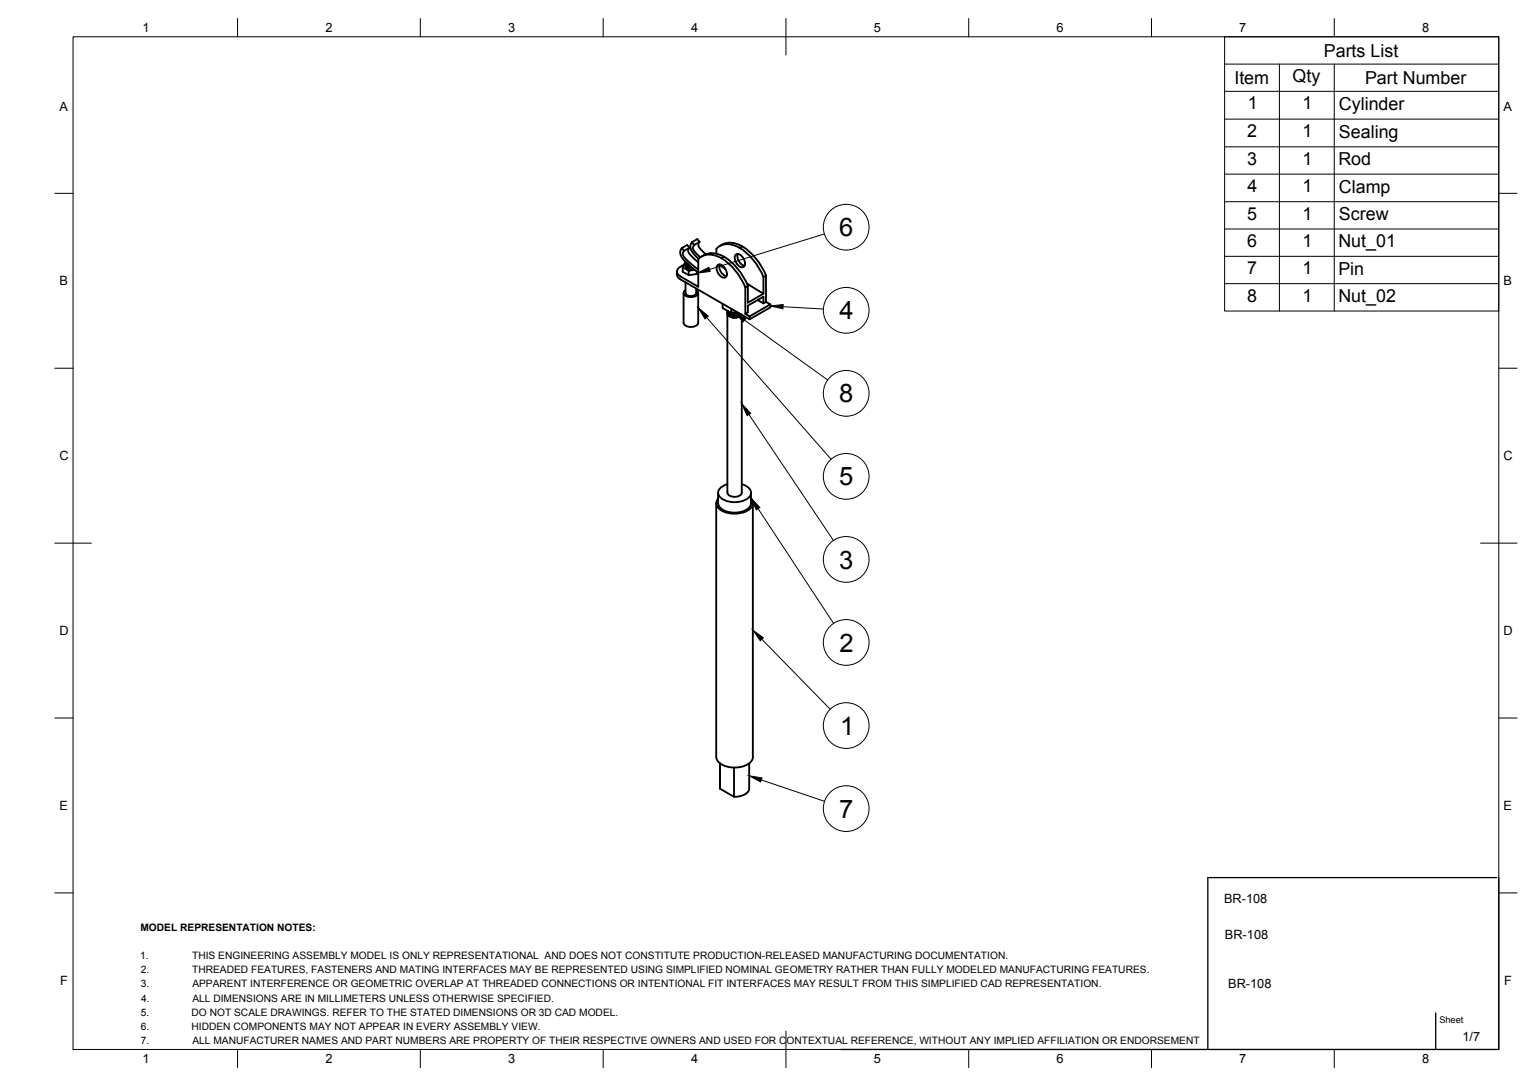
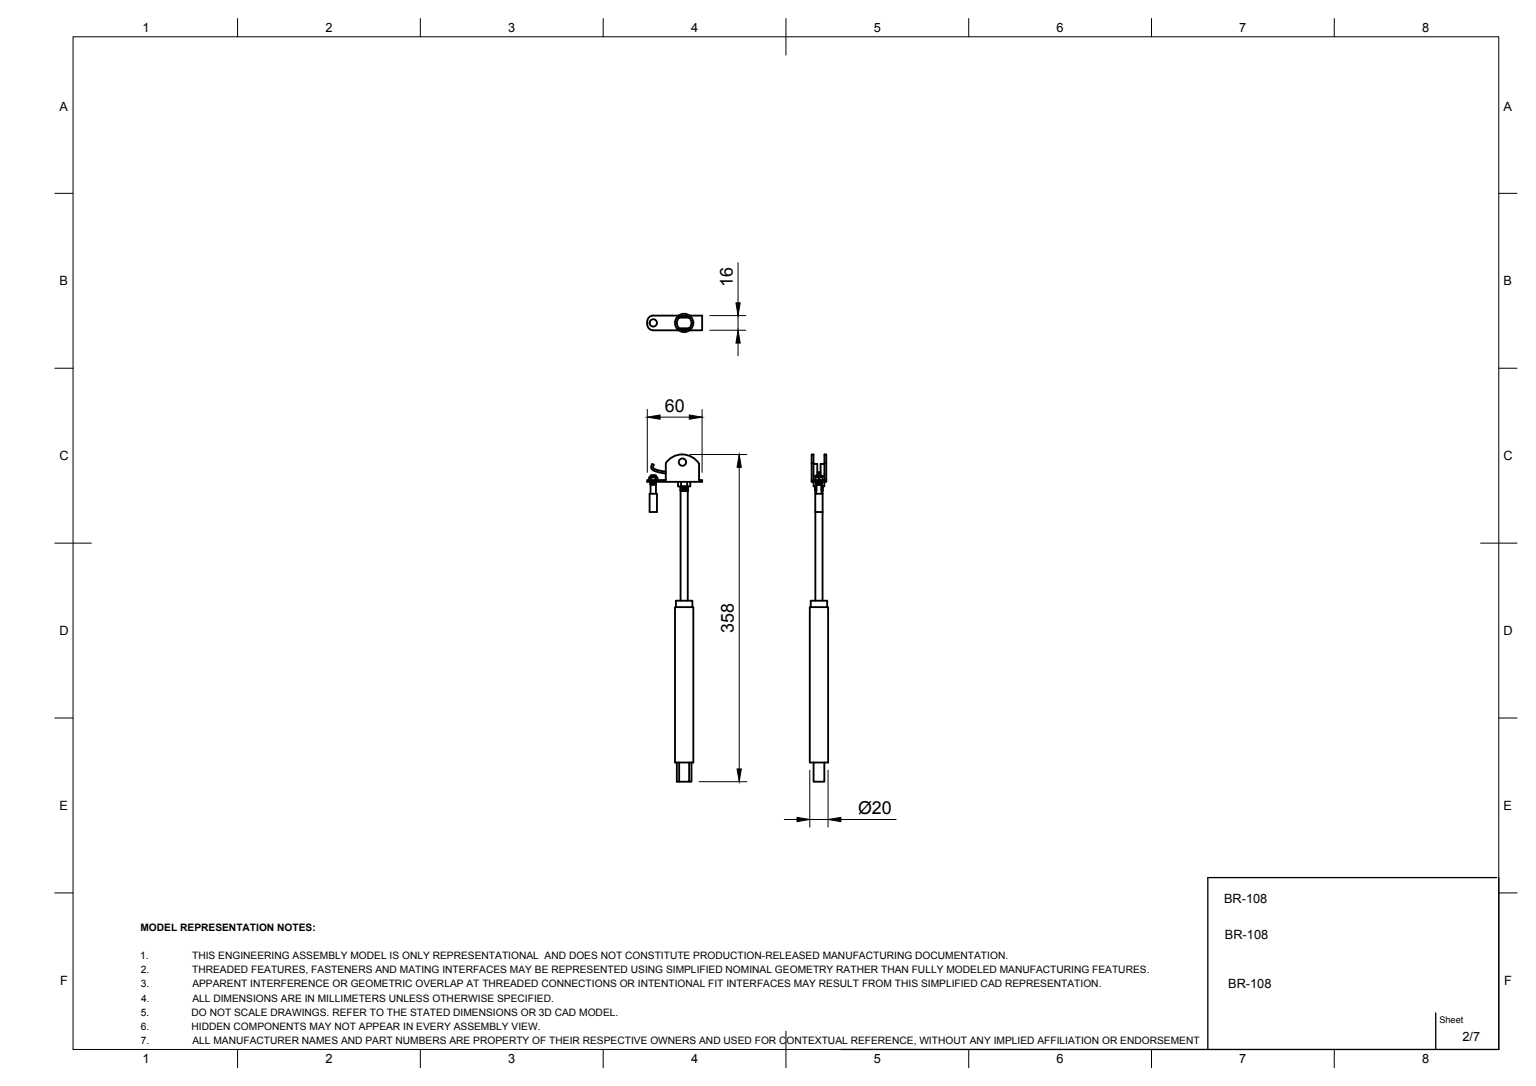
ISO-10303-21;
HEADER;
/* Generated by software containing ST-Developer
 * from STEP Tools, Inc. (www.steptools.com) 
 */

FILE_DESCRIPTION(
/* description */ (''),
/* implementation_level */ '2;1');

FILE_NAME(
/* name */ 'BR-108.step',
/* time_stamp */ '2026-11-14T03:52:36-08:00',
/* author */ (''),
/* organization */ (''),
/* preprocessor_version */ 'ST-DEVELOPER v20.2',
/* originating_system */ 'Autodesk Translation Framework v15.17.0.0',
/* authorisation */ '');

FILE_SCHEMA (('AUTOMOTIVE_DESIGN { 1 0 10303 214 3 1 1 }'));
ENDSEC;

DATA;
#10=MECHANICAL_DESIGN_GEOMETRIC_PRESENTATION_REPRESENTATION('',(#191,#192,
#193,#194,#195,#196,#197,#198),#19443);
#11=ITEM_DEFINED_TRANSFORMATION($,$,#2116,#2258);
#12=ITEM_DEFINED_TRANSFORMATION($,$,#2125,#2259);
#13=ITEM_DEFINED_TRANSFORMATION($,$,#2131,#2260);
#14=ITEM_DEFINED_TRANSFORMATION($,$,#2150,#2261);
#15=ITEM_DEFINED_TRANSFORMATION($,$,#2195,#2262);
#16=ITEM_DEFINED_TRANSFORMATION($,$,#2220,#2263);
#17=ITEM_DEFINED_TRANSFORMATION($,$,#2232,#2264);
#18=ITEM_DEFINED_TRANSFORMATION($,$,#2246,#2265);
#19=(
REPRESENTATION_RELATIONSHIP($,$,#19475,#19474)
REPRESENTATION_RELATIONSHIP_WITH_TRANSFORMATION(#11)
SHAPE_REPRESENTATION_RELATIONSHIP()
);
#20=(
REPRESENTATION_RELATIONSHIP($,$,#19476,#19474)
REPRESENTATION_RELATIONSHIP_WITH_TRANSFORMATION(#12)
SHAPE_REPRESENTATION_RELATIONSHIP()
);
#21=(
REPRESENTATION_RELATIONSHIP($,$,#19477,#19474)
REPRESENTATION_RELATIONSHIP_WITH_TRANSFORMATION(#13)
SHAPE_REPRESENTATION_RELATIONSHIP()
);
#22=(
REPRESENTATION_RELATIONSHIP($,$,#19478,#19474)
REPRESENTATION_RELATIONSHIP_WITH_TRANSFORMATION(#14)
SHAPE_REPRESENTATION_RELATIONSHIP()
);
#23=(
REPRESENTATION_RELATIONSHIP($,$,#19479,#19474)
REPRESENTATION_RELATIONSHIP_WITH_TRANSFORMATION(#15)
SHAPE_REPRESENTATION_RELATIONSHIP()
);
#24=(
REPRESENTATION_RELATIONSHIP($,$,#19480,#19474)
REPRESENTATION_RELATIONSHIP_WITH_TRANSFORMATION(#16)
SHAPE_REPRESENTATION_RELATIONSHIP()
);
#25=(
REPRESENTATION_RELATIONSHIP($,$,#19481,#19474)
REPRESENTATION_RELATIONSHIP_WITH_TRANSFORMATION(#17)
SHAPE_REPRESENTATION_RELATIONSHIP()
);
#26=(
REPRESENTATION_RELATIONSHIP($,$,#19482,#19474)
REPRESENTATION_RELATIONSHIP_WITH_TRANSFORMATION(#18)
SHAPE_REPRESENTATION_RELATIONSHIP()
);
#27=CONTEXT_DEPENDENT_SHAPE_REPRESENTATION(#19,#19466);
#28=CONTEXT_DEPENDENT_SHAPE_REPRESENTATION(#20,#19467);
#29=CONTEXT_DEPENDENT_SHAPE_REPRESENTATION(#21,#19468);
#30=CONTEXT_DEPENDENT_SHAPE_REPRESENTATION(#22,#19469);
#31=CONTEXT_DEPENDENT_SHAPE_REPRESENTATION(#23,#19470);
#32=CONTEXT_DEPENDENT_SHAPE_REPRESENTATION(#24,#19471);
#33=CONTEXT_DEPENDENT_SHAPE_REPRESENTATION(#25,#19472);
#34=CONTEXT_DEPENDENT_SHAPE_REPRESENTATION(#26,#19473);
#35=NEXT_ASSEMBLY_USAGE_OCCURRENCE('Cylinder:1','Cylinder:1',
'Cylinder:1',#19484,#19485,'Cylinder:1');
#36=NEXT_ASSEMBLY_USAGE_OCCURRENCE('Sealing:1','Sealing:1','Sealing:1',
#19484,#19486,'Sealing:1');
#37=NEXT_ASSEMBLY_USAGE_OCCURRENCE('Rod:1','Rod:1','Rod:1',#19484,#19487,
'Rod:1');
#38=NEXT_ASSEMBLY_USAGE_OCCURRENCE('Clamp:1','Clamp:1','Clamp:1',#19484,
#19488,'Clamp:1');
#39=NEXT_ASSEMBLY_USAGE_OCCURRENCE('Screw:1','Screw:1','Screw:1',#19484,
#19489,'Screw:1');
#40=NEXT_ASSEMBLY_USAGE_OCCURRENCE('Nut_01:1','Nut_01:1','Nut_01:1',#19484,
#19490,'Nut_01:1');
#41=NEXT_ASSEMBLY_USAGE_OCCURRENCE('Pin:1','Pin:1','Pin:1',#19484,#19491,
'Pin:1');
#42=NEXT_ASSEMBLY_USAGE_OCCURRENCE('Nut_02:1','Nut_02:1','Nut_02:1',#19484,
#19492,'Nut_02:1');
#43=B_SPLINE_SURFACE_WITH_KNOTS('',3,3,((#8954,#8955,#8956,#8957,#8958,
#8959,#8960,#8961,#8962,#8963,#8964,#8965,#8966,#8967,#8968,#8969,#8970,
#8971,#8972,#8973,#8974,#8975,#8976,#8977,#8978,#8979,#8980,#8981,#8982,
#8983,#8984,#8985,#8986,#8987,#8988,#8989,#8990,#8991,#8992,#8993,#8994,
#8995,#8996,#8997,#8998,#8999,#9000,#9001,#9002,#9003,#9004,#9005,#9006,
#9007,#9008,#9009),(#9010,#9011,#9012,#9013,#9014,#9015,#9016,#9017,#9018,
#9019,#9020,#9021,#9022,#9023,#9024,#9025,#9026,#9027,#9028,#9029,#9030,
#9031,#9032,#9033,#9034,#9035,#9036,#9037,#9038,#9039,#9040,#9041,#9042,
#9043,#9044,#9045,#9046,#9047,#9048,#9049,#9050,#9051,#9052,#9053,#9054,
#9055,#9056,#9057,#9058,#9059,#9060,#9061,#9062,#9063,#9064,#9065),(#9066,
#9067,#9068,#9069,#9070,#9071,#9072,#9073,#9074,#9075,#9076,#9077,#9078,
#9079,#9080,#9081,#9082,#9083,#9084,#9085,#9086,#9087,#9088,#9089,#9090,
#9091,#9092,#9093,#9094,#9095,#9096,#9097,#9098,#9099,#9100,#9101,#9102,
#9103,#9104,#9105,#9106,#9107,#9108,#9109,#9110,#9111,#9112,#9113,#9114,
#9115,#9116,#9117,#9118,#9119,#9120,#9121),(#9122,#9123,#9124,#9125,#9126,
#9127,#9128,#9129,#9130,#9131,#9132,#9133,#9134,#9135,#9136,#9137,#9138,
#9139,#9140,#9141,#9142,#9143,#9144,#9145,#9146,#9147,#9148,#9149,#9150,
#9151,#9152,#9153,#9154,#9155,#9156,#9157,#9158,#9159,#9160,#9161,#9162,
#9163,#9164,#9165,#9166,#9167,#9168,#9169,#9170,#9171,#9172,#9173,#9174,
#9175,#9176,#9177)),.UNSPECIFIED.,.F.,.F.,.F.,(4,4),(4,1,1,1,1,1,1,1,1,
1,1,1,1,1,1,1,1,1,1,1,1,1,1,1,1,1,1,1,1,1,1,1,1,1,1,1,1,1,1,1,1,1,1,1,1,
1,1,1,1,1,1,1,1,4),(-0.000657437329809864,0.0823479142293904),(8.31473274985805,
9.30202867542319,10.2893246009883,11.2766205265535,12.2639164521186,13.2512123776837,
14.2385083032489,15.225804228814,16.2131001543792,17.2003960799443,18.1876920055094,
19.1749879310746,20.1622838566397,21.1495797822049,22.13687570777,23.1241716333351,
24.1114675589003,25.0987634844654,26.0860594100306,27.0733553355957,28.0606512611608,
29.047947186726,30.0352431122911,31.0225390378563,32.0098349634214,32.9971308889865,
33.9844268145517,34.9717227401168,35.959018665682,36.9463145912471,37.9336105168122,
38.9209064423774,39.9082023679425,40.8954982935077,41.8827942190728,42.8700901446379,
43.8573860702031,44.8446819957682,45.8319779213334,46.8192738468985,47.8065697724636,
48.7938656980288,49.7811616235939,50.7684575491591,51.7557534747242,52.7430494002893,
53.7303453258545,54.7176412514196,55.7049371769848,56.6922331025499,57.679529028115,
58.6668249536802,59.6541208792453,60.6420742421403),.UNSPECIFIED.);
#44=B_SPLINE_SURFACE_WITH_KNOTS('',3,3,((#9461,#9462,#9463,#9464,#9465,
#9466,#9467,#9468,#9469,#9470,#9471,#9472,#9473,#9474,#9475,#9476,#9477,
#9478,#9479,#9480,#9481,#9482,#9483,#9484,#9485,#9486,#9487,#9488,#9489,
#9490,#9491,#9492,#9493,#9494,#9495,#9496,#9497,#9498,#9499,#9500,#9501,
#9502,#9503,#9504,#9505,#9506,#9507,#9508,#9509,#9510,#9511,#9512,#9513,
#9514,#9515,#9516),(#9517,#9518,#9519,#9520,#9521,#9522,#9523,#9524,#9525,
#9526,#9527,#9528,#9529,#9530,#9531,#9532,#9533,#9534,#9535,#9536,#9537,
#9538,#9539,#9540,#9541,#9542,#9543,#9544,#9545,#9546,#9547,#9548,#9549,
#9550,#9551,#9552,#9553,#9554,#9555,#9556,#9557,#9558,#9559,#9560,#9561,
#9562,#9563,#9564,#9565,#9566,#9567,#9568,#9569,#9570,#9571,#9572),(#9573,
#9574,#9575,#9576,#9577,#9578,#9579,#9580,#9581,#9582,#9583,#9584,#9585,
#9586,#9587,#9588,#9589,#9590,#9591,#9592,#9593,#9594,#9595,#9596,#9597,
#9598,#9599,#9600,#9601,#9602,#9603,#9604,#9605,#9606,#9607,#9608,#9609,
#9610,#9611,#9612,#9613,#9614,#9615,#9616,#9617,#9618,#9619,#9620,#9621,
#9622,#9623,#9624,#9625,#9626,#9627,#9628),(#9629,#9630,#9631,#9632,#9633,
#9634,#9635,#9636,#9637,#9638,#9639,#9640,#9641,#9642,#9643,#9644,#9645,
#9646,#9647,#9648,#9649,#9650,#9651,#9652,#9653,#9654,#9655,#9656,#9657,
#9658,#9659,#9660,#9661,#9662,#9663,#9664,#9665,#9666,#9667,#9668,#9669,
#9670,#9671,#9672,#9673,#9674,#9675,#9676,#9677,#9678,#9679,#9680,#9681,
#9682,#9683,#9684)),.UNSPECIFIED.,.F.,.F.,.F.,(4,4),(4,1,1,1,1,1,1,1,1,
1,1,1,1,1,1,1,1,1,1,1,1,1,1,1,1,1,1,1,1,1,1,1,1,1,1,1,1,1,1,1,1,1,1,1,1,
1,1,1,1,1,1,1,1,4),(-0.00040521448804481,0.0826859266002323),(11.6145409068929,
12.6025101533199,13.589806078885,14.5771020044501,15.5643979300153,16.5516938555804,
17.5389897811456,18.5262857067107,19.5135816322758,20.500877557841,21.4881734834061,
22.4754694089713,23.4627653345364,24.4500612601015,25.4373571856667,26.4246531112318,
27.411949036797,28.3992449623621,29.3865408879273,30.3738368134924,31.3611327390575,
32.3484286646227,33.3357245901878,34.323020515753,35.3103164413181,36.2976123668832,
37.2849082924484,38.2722042180135,39.2595001435787,40.2467960691438,41.2340919947089,
42.2213879202741,43.2086838458392,44.1959797714044,45.1832756969695,46.1705716225347,
47.1578675480998,48.1451634736649,49.1324593992301,50.1197553247952,51.1070512503604,
52.0943471759255,53.0816431014906,54.0689390270558,55.0562349526209,56.0435308781861,
57.0308268037512,58.0181227293163,59.0054186548815,59.9927145804466,60.9800105060118,
61.9673064315769,62.954602357142,63.9418982827072),.UNSPECIFIED.);
#45=B_SPLINE_SURFACE_WITH_KNOTS('',5,1,((#10544,#10545),(#10546,#10547),
(#10548,#10549),(#10550,#10551),(#10552,#10553),(#10554,#10555),(#10556,
#10557),(#10558,#10559),(#10560,#10561),(#10562,#10563),(#10564,#10565),
(#10566,#10567),(#10568,#10569),(#10570,#10571),(#10572,#10573),(#10574,
#10575),(#10576,#10577),(#10578,#10579),(#10580,#10581),(#10582,#10583),
(#10584,#10585),(#10586,#10587),(#10588,#10589),(#10590,#10591),(#10592,
#10593)),.UNSPECIFIED.,.F.,.F.,.F.,(6,1,1,1,1,1,1,1,1,1,1,1,1,1,1,1,1,1,
1,1,6),(2,2),(0.,0.05,0.1,0.15,0.2,0.25,0.3,0.35,0.4,0.45,0.5,0.55,0.6,
0.65,0.7,0.75,0.8,0.85,0.9,0.95,0.997783576468117),(0.,2.28),
 .UNSPECIFIED.);
#46=B_SPLINE_SURFACE_WITH_KNOTS('',3,1,((#10795,#10796),(#10797,#10798),
(#10799,#10800),(#10801,#10802),(#10803,#10804),(#10805,#10806),(#10807,
#10808),(#10809,#10810),(#10811,#10812),(#10813,#10814),(#10815,#10816),
(#10817,#10818),(#10819,#10820),(#10821,#10822),(#10823,#10824),(#10825,
#10826),(#10827,#10828),(#10829,#10830),(#10831,#10832),(#10833,#10834),
(#10835,#10836),(#10837,#10838)),.UNSPECIFIED.,.F.,.F.,.F.,(4,3,3,3,3,3,
3,4),(2,2),(-1.,-0.911417181577933,-0.82714074028049,-0.742907558806874,
-0.633245293286216,-0.436057375062027,-0.250000004296482,-0.000486150394329065),
(0.,2.28),.UNSPECIFIED.);
#47=B_SPLINE_SURFACE_WITH_KNOTS('',3,3,((#18367,#18368,#18369,#18370,#18371,
#18372,#18373,#18374,#18375,#18376,#18377,#18378,#18379,#18380,#18381,#18382,
#18383,#18384,#18385,#18386,#18387,#18388,#18389,#18390,#18391,#18392,#18393,
#18394,#18395,#18396,#18397,#18398,#18399,#18400,#18401,#18402,#18403,#18404,
#18405,#18406,#18407,#18408,#18409,#18410,#18411,#18412,#18413,#18414,#18415,
#18416,#18417,#18418,#18419,#18420,#18421,#18422,#18423,#18424,#18425,#18426,
#18427,#18428,#18429,#18430,#18431,#18432,#18433,#18434),(#18435,#18436,
#18437,#18438,#18439,#18440,#18441,#18442,#18443,#18444,#18445,#18446,#18447,
#18448,#18449,#18450,#18451,#18452,#18453,#18454,#18455,#18456,#18457,#18458,
#18459,#18460,#18461,#18462,#18463,#18464,#18465,#18466,#18467,#18468,#18469,
#18470,#18471,#18472,#18473,#18474,#18475,#18476,#18477,#18478,#18479,#18480,
#18481,#18482,#18483,#18484,#18485,#18486,#18487,#18488,#18489,#18490,#18491,
#18492,#18493,#18494,#18495,#18496,#18497,#18498,#18499,#18500,#18501,#18502),
(#18503,#18504,#18505,#18506,#18507,#18508,#18509,#18510,#18511,#18512,
#18513,#18514,#18515,#18516,#18517,#18518,#18519,#18520,#18521,#18522,#18523,
#18524,#18525,#18526,#18527,#18528,#18529,#18530,#18531,#18532,#18533,#18534,
#18535,#18536,#18537,#18538,#18539,#18540,#18541,#18542,#18543,#18544,#18545,
#18546,#18547,#18548,#18549,#18550,#18551,#18552,#18553,#18554,#18555,#18556,
#18557,#18558,#18559,#18560,#18561,#18562,#18563,#18564,#18565,#18566,#18567,
#18568,#18569,#18570),(#18571,#18572,#18573,#18574,#18575,#18576,#18577,
#18578,#18579,#18580,#18581,#18582,#18583,#18584,#18585,#18586,#18587,#18588,
#18589,#18590,#18591,#18592,#18593,#18594,#18595,#18596,#18597,#18598,#18599,
#18600,#18601,#18602,#18603,#18604,#18605,#18606,#18607,#18608,#18609,#18610,
#18611,#18612,#18613,#18614,#18615,#18616,#18617,#18618,#18619,#18620,#18621,
#18622,#18623,#18624,#18625,#18626,#18627,#18628,#18629,#18630,#18631,#18632,
#18633,#18634,#18635,#18636,#18637,#18638)),.UNSPECIFIED.,.F.,.F.,.F.,(4,
4),(4,1,1,1,1,1,1,1,1,1,1,1,1,1,1,1,1,1,1,1,1,1,1,1,1,1,1,1,1,1,1,1,1,1,
1,1,1,1,1,1,1,1,1,1,1,1,1,1,1,1,1,1,1,1,1,1,1,1,1,1,1,1,1,1,1,4),(-0.000501830952949241,
0.0663068519672736),(8.30747755240111,9.30594664850426,10.3044157446074,
11.3028848407106,12.3013539368137,13.2998230329169,14.29829212902,15.2967612251232,
16.2952303212263,17.2936994173295,18.2921685134326,19.2906376095358,20.2891067056389,
21.2875758017421,22.2860448978452,23.2845139939484,24.2829830900515,25.2814521861547,
26.2799212822578,27.278390378361,28.2768594744641,29.2753285705673,30.2737976666704,
31.2722667627736,32.2707358588767,33.2692049549799,34.267674051083,35.2661431471862,
36.2646122432893,37.2630813393925,38.2615504354956,39.2600195315988,40.258488627702,
41.2569577238051,42.2554268199083,43.2538959160114,44.2523650121146,45.2508341082177,
46.2493032043209,47.247772300424,48.2462413965272,49.2447104926303,50.2431795887335,
51.2416486848366,52.2401177809398,53.2385868770429,54.2370559731461,55.2355250692492,
56.2339941653524,57.2324632614555,58.2309323575587,59.2294014536618,60.227870549765,
61.2263396458681,62.2248087419713,63.2232778380744,64.2217469341776,65.2202160302807,
66.2186851263839,67.217154222487,68.2156233185902,69.2140924146934,70.2125615107965,
71.2110306068997,72.2094997030028,73.208470630059),.UNSPECIFIED.);
#48=B_SPLINE_SURFACE_WITH_KNOTS('',3,3,((#18916,#18917,#18918,#18919,#18920,
#18921,#18922,#18923,#18924,#18925,#18926,#18927,#18928,#18929,#18930,#18931,
#18932,#18933,#18934,#18935,#18936,#18937,#18938,#18939,#18940,#18941,#18942,
#18943,#18944,#18945,#18946,#18947,#18948,#18949,#18950,#18951,#18952,#18953,
#18954,#18955,#18956,#18957,#18958,#18959,#18960,#18961,#18962,#18963,#18964,
#18965,#18966,#18967,#18968,#18969,#18970,#18971,#18972,#18973,#18974,#18975,
#18976,#18977,#18978,#18979,#18980,#18981,#18982,#18983),(#18984,#18985,
#18986,#18987,#18988,#18989,#18990,#18991,#18992,#18993,#18994,#18995,#18996,
#18997,#18998,#18999,#19000,#19001,#19002,#19003,#19004,#19005,#19006,#19007,
#19008,#19009,#19010,#19011,#19012,#19013,#19014,#19015,#19016,#19017,#19018,
#19019,#19020,#19021,#19022,#19023,#19024,#19025,#19026,#19027,#19028,#19029,
#19030,#19031,#19032,#19033,#19034,#19035,#19036,#19037,#19038,#19039,#19040,
#19041,#19042,#19043,#19044,#19045,#19046,#19047,#19048,#19049,#19050,#19051),
(#19052,#19053,#19054,#19055,#19056,#19057,#19058,#19059,#19060,#19061,
#19062,#19063,#19064,#19065,#19066,#19067,#19068,#19069,#19070,#19071,#19072,
#19073,#19074,#19075,#19076,#19077,#19078,#19079,#19080,#19081,#19082,#19083,
#19084,#19085,#19086,#19087,#19088,#19089,#19090,#19091,#19092,#19093,#19094,
#19095,#19096,#19097,#19098,#19099,#19100,#19101,#19102,#19103,#19104,#19105,
#19106,#19107,#19108,#19109,#19110,#19111,#19112,#19113,#19114,#19115,#19116,
#19117,#19118,#19119),(#19120,#19121,#19122,#19123,#19124,#19125,#19126,
#19127,#19128,#19129,#19130,#19131,#19132,#19133,#19134,#19135,#19136,#19137,
#19138,#19139,#19140,#19141,#19142,#19143,#19144,#19145,#19146,#19147,#19148,
#19149,#19150,#19151,#19152,#19153,#19154,#19155,#19156,#19157,#19158,#19159,
#19160,#19161,#19162,#19163,#19164,#19165,#19166,#19167,#19168,#19169,#19170,
#19171,#19172,#19173,#19174,#19175,#19176,#19177,#19178,#19179,#19180,#19181,
#19182,#19183,#19184,#19185,#19186,#19187)),.UNSPECIFIED.,.F.,.F.,.F.,(4,
4),(4,1,1,1,1,1,1,1,1,1,1,1,1,1,1,1,1,1,1,1,1,1,1,1,1,1,1,1,1,1,1,1,1,1,
1,1,1,1,1,1,1,1,1,1,1,1,1,1,1,1,1,1,1,1,1,1,1,1,1,1,1,1,1,1,1,4),(-0.000439241290791206,
0.0663646041699065),(11.6145150418495,12.6135019439215,13.6119710400246,
14.6104401361278,15.6089092322309,16.6073783283341,17.6058474244372,18.6043165205404,
19.6027856166435,20.6012547127467,21.5997238088498,22.598192904953,23.5966620010561,
24.5951310971593,25.5936001932624,26.5920692893656,27.5905383854687,28.5890074815719,
29.5874765776751,30.5859456737782,31.5844147698814,32.5828838659845,33.5813529620877,
34.5798220581908,35.578291154294,36.5767602503971,37.5752293465003,38.5736984426034,
39.5721675387066,40.5706366348097,41.5691057309129,42.567574827016,43.5660439231192,
44.5645130192223,45.5629821153255,46.5614512114286,47.5599203075318,48.5583894036349,
49.5568584997381,50.5553275958412,51.5537966919444,52.5522657880475,53.5507348841507,
54.5492039802538,55.547673076357,56.5461421724601,57.5446112685633,58.5430803646665,
59.5415494607696,60.5400185568728,61.5384876529759,62.5369567490791,63.5354258451822,
64.5338949412854,65.5323640373885,66.5308331334917,67.5293022295948,68.527771325698,
69.5262404218011,70.5247095179043,71.5231786140074,72.5216477101106,73.5201168062137,
74.5185859023169,75.51705499842,76.5155240945232),.UNSPECIFIED.);
#49=B_SPLINE_CURVE_WITH_KNOTS('',3,(#2726,#2727,#2728,#2729,#2730,#2731,
#2732,#2733,#2734,#2735,#2736,#2737,#2738,#2739,#2740,#2741,#2742,#2743,
#2744,#2745,#2746,#2747,#2748,#2749,#2750,#2751,#2752,#2753,#2754,#2755,
#2756,#2757,#2758,#2759,#2760,#2761,#2762,#2763,#2764,#2765,#2766,#2767,
#2768,#2769,#2770,#2771,#2772,#2773,#2774,#2775,#2776,#2777,#2778,#2779,
#2780,#2781,#2782,#2783,#2784,#2785,#2786,#2787,#2788,#2789,#2790,#2791,
#2792,#2793,#2794,#2795,#2796,#2797,#2798,#2799,#2800,#2801,#2802,#2803,
#2804,#2805,#2806,#2807,#2808,#2809,#2810,#2811,#2812,#2813,#2814,#2815,
#2816,#2817,#2818,#2819,#2820,#2821,#2822,#2823,#2824,#2825,#2826,#2827,
#2828,#2829,#2830,#2831,#2832,#2833,#2834,#2835,#2836,#2837),
 .UNSPECIFIED.,.F.,.F.,(4,3,3,3,3,3,3,3,3,3,3,3,3,3,3,3,3,3,3,3,3,3,3,3,
3,3,3,3,3,3,3,3,3,3,3,3,3,4),(10.3764175401129,10.4684762321019,10.560419481767,
10.6522725450313,10.7440770571527,10.8358588565194,10.9276437548813,11.0195141021843,
11.1114281051697,11.2034893563628,11.2766205265535,11.3699699521422,11.4631985738672,
11.5563335991914,11.6494062321449,11.7424472221572,11.8354810277323,11.9285320946886,
12.0216816252994,12.11488490924,12.2082354140953,12.2639164521186,12.3570693480044,
12.4500982166783,12.5430305679426,12.6358970169529,12.7287297400997,12.8215534563738,
12.9143928706346,13.0073296432903,13.1003192457673,13.1934566991756,13.2512123776837,
13.3444476686996,13.4375356185427,13.5305385459024,13.6234740197825,13.6618555532241),
 .UNSPECIFIED.);
#50=B_SPLINE_CURVE_WITH_KNOTS('',3,(#2840,#2841,#2842,#2843,#2844,#2845,
#2846,#2847,#2848,#2849,#2850,#2851,#2852,#2853,#2854,#2855,#2856,#2857,
#2858,#2859,#2860,#2861,#2862,#2863,#2864,#2865,#2866,#2867,#2868,#2869,
#2870,#2871,#2872,#2873,#2874,#2875,#2876,#2877,#2878,#2879,#2880,#2881,
#2882,#2883,#2884,#2885,#2886,#2887,#2888,#2889,#2890,#2891,#2892,#2893,
#2894,#2895,#2896,#2897),.UNSPECIFIED.,.F.,.F.,(4,2,2,2,2,2,2,2,2,2,2,2,
2,2,2,2,2,2,2,2,2,2,2,2,2,2,2,2,4),(-3.35276873050689,-3.34541163931656,
-3.33454410942102,-3.28988621968237,-3.2367451420787,-3.21797771526182,
-3.20584415076294,-3.19380116055654,-3.17568959207908,-3.10036172591383,
-3.06621207860194,-3.05209120789862,-3.04101266877526,-3.03450717101804,
-3.02822963770033,-3.01796361528236,-2.95640611952485,-2.90263005834274,
-2.88767690300836,-2.87719641995359,-2.86629447482556,-2.84906124499233,
-2.78107728025335,-2.72943250313414,-2.7194202959918,-2.71333138514061,
-2.70696516579511,-2.6963401900384,-2.69172026756216),.UNSPECIFIED.);
#51=B_SPLINE_CURVE_WITH_KNOTS('',3,(#2903,#2904,#2905,#2906,#2907,#2908,
#2909,#2910,#2911,#2912,#2913,#2914,#2915,#2916,#2917,#2918,#2919,#2920,
#2921,#2922,#2923,#2924,#2925,#2926,#2927,#2928,#2929,#2930,#2931,#2932,
#2933,#2934,#2935,#2936,#2937,#2938,#2939,#2940,#2941,#2942,#2943,#2944,
#2945,#2946,#2947,#2948,#2949,#2950,#2951,#2952,#2953,#2954,#2955,#2956,
#2957,#2958,#2959,#2960,#2961,#2962,#2963,#2964,#2965,#2966,#2967,#2968,
#2969,#2970,#2971,#2972,#2973,#2974,#2975,#2976,#2977,#2978,#2979,#2980,
#2981,#2982,#2983,#2984,#2985,#2986,#2987,#2988,#2989,#2990,#2991,#2992,
#2993,#2994,#2995,#2996,#2997,#2998,#2999,#3000,#3001,#3002,#3003,#3004,
#3005,#3006,#3007,#3008,#3009,#3010,#3011,#3012,#3013,#3014,#3015,#3016,
#3017,#3018),.UNSPECIFIED.,.F.,.F.,(4,2,2,2,2,2,2,2,2,2,2,2,2,2,2,2,2,2,
2,2,2,2,2,2,2,2,2,2,2,2,2,2,2,2,2,2,2,2,2,2,2,2,2,2,2,2,2,2,2,2,2,2,2,2,
2,2,2,4),(-1.36964803891745,-1.30750439248835,-1.29117702151389,-1.28131054610571,
-1.27046681979769,-1.25480347710278,-1.19411610031767,-1.13876432373534,
-1.12764923556203,-1.12116620037127,-1.11483314340789,-1.10444786024198,
-1.09141491148914,-1.06110808838298,-0.988304024651697,-0.972093214280928,
-0.962245862176411,-0.951384177567935,-0.93561404698589,-0.876136217249594,
-0.819739530316951,-0.808663581702881,-0.802188694069041,-0.795848406891141,
-0.785428692256478,-0.772337850319824,-0.741796767684607,-0.669493053605558,
-0.653213006000507,-0.643353819682297,-0.632501979477615,-0.61679356347468,
-0.598449431655796,-0.560112935304642,-0.500216729476669,-0.489459341196301,
-0.483049710050318,-0.476646785775137,-0.465925187741241,-0.452320896136076,
-0.419631521650988,-0.351744719600656,-0.334921971516567,-0.323870468080585,
-0.312913218242703,-0.296609562925145,-0.237881919328277,-0.18192230055348,
-0.170826288952788,-0.164346905178106,-0.15801332963989,-0.147617386068845,
-0.134565346412738,-0.104177970967796,-0.0340764265464484,-0.0169290231420096,
-0.00796895088548166,-0.000909006770802341),.UNSPECIFIED.);
#52=B_SPLINE_CURVE_WITH_KNOTS('',3,(#3019,#3020,#3021,#3022,#3023,#3024,
#3025,#3026,#3027,#3028,#3029,#3030,#3031,#3032,#3033,#3034,#3035,#3036,
#3037,#3038,#3039,#3040,#3041,#3042,#3043,#3044,#3045,#3046,#3047,#3048,
#3049,#3050,#3051,#3052,#3053,#3054,#3055,#3056,#3057,#3058,#3059,#3060,
#3061,#3062,#3063,#3064,#3065,#3066,#3067,#3068,#3069,#3070,#3071,#3072,
#3073,#3074,#3075,#3076,#3077,#3078,#3079,#3080,#3081,#3082,#3083,#3084,
#3085,#3086,#3087,#3088),.UNSPECIFIED.,.F.,.F.,(4,3,3,3,3,3,3,3,3,3,3,3,
3,3,3,3,3,3,3,3,3,3,3,4),(13.6618555532241,13.7547559501353,13.8476578284241,
13.9453704471303,14.0384037073382,14.1315001278033,14.2247319191675,14.2385083032489,
14.3317395576815,14.4248478824819,14.5178606701666,14.6108086845596,14.7037236383471,
14.7966301491715,14.8895528209867,14.9825730552894,15.0756463542335,15.1688670547424,
15.225804228814,15.3242048935619,15.422335295086,15.5203045747014,15.6180521915914,
15.7079632677538),.UNSPECIFIED.);
#53=B_SPLINE_CURVE_WITH_KNOTS('',3,(#3089,#3090,#3091,#3092,#3093,#3094,
#3095,#3096,#3097,#3098,#3099,#3100,#3101,#3102,#3103,#3104,#3105,#3106,
#3107,#3108,#3109,#3110,#3111,#3112,#3113,#3114,#3115,#3116,#3117,#3118,
#3119,#3120,#3121,#3122,#3123,#3124,#3125,#3126,#3127,#3128,#3129,#3130,
#3131,#3132,#3133,#3134,#3135,#3136,#3137,#3138,#3139,#3140,#3141,#3142,
#3143,#3144,#3145,#3146,#3147,#3148,#3149,#3150,#3151,#3152,#3153,#3154,
#3155,#3156,#3157,#3158,#3159,#3160,#3161,#3162,#3163,#3164,#3165,#3166,
#3167,#3168,#3169,#3170,#3171,#3172,#3173,#3174,#3175,#3176,#3177,#3178,
#3179,#3180,#3181,#3182,#3183,#3184,#3185,#3186,#3187,#3188,#3189,#3190,
#3191,#3192,#3193,#3194,#3195,#3196,#3197,#3198,#3199,#3200,#3201,#3202,
#3203,#3204,#3205,#3206,#3207,#3208,#3209,#3210,#3211,#3212,#3213,#3214,
#3215,#3216,#3217,#3218,#3219,#3220,#3221,#3222,#3223,#3224,#3225,#3226,
#3227,#3228,#3229,#3230,#3231,#3232,#3233,#3234,#3235,#3236,#3237,#3238,
#3239,#3240,#3241,#3242,#3243,#3244,#3245,#3246,#3247,#3248),
 .UNSPECIFIED.,.F.,.F.,(4,2,2,2,2,2,2,2,2,2,2,2,2,2,2,2,2,2,2,2,2,2,2,2,
2,2,2,2,2,2,2,2,2,2,2,2,2,2,2,2,2,2,2,2,2,2,2,2,2,2,2,2,2,2,2,2,2,2,2,2,
2,2,2,2,2,2,2,2,2,2,2,2,2,2,2,2,2,2,2,4),(-2.69172026756216,-2.6352719778585,
-2.58053932952011,-2.56403952316667,-2.55298302906342,-2.54184725993664,
-2.52489765210718,-2.46049400488895,-2.4134571930637,-2.40261993901256,
-2.39612873883492,-2.3896297153635,-2.37859563248551,-2.32113463283633,
-2.26300703893396,-2.24709631499146,-2.23615960029177,-2.2262535246208,
-2.20995871418767,-2.13731879481618,-2.10689703379286,-2.09381670889935,
-2.08339320333483,-2.07703103205796,-2.07055590922739,-2.05943586161933,
-2.00451879050627,-1.94524564423088,-1.92879744188377,-1.91784270207866,
-1.90687315290747,-1.89034526278203,-1.81964968414538,-1.77336629031843,
-1.76352733265447,-1.75731584664119,-1.75069706235437,-1.73893559740849,
-1.67703680599441,-1.62753135510787,-1.61022061477051,-1.59906379949906,
-1.58815412521391,-1.57220494550319,-1.55348415739971,-1.51368071751401,
-1.45693404941784,-1.44588190611916,-1.43940053463916,-1.43303563482373,
-1.4225301442536,-1.37391976247168,-1.30842245398281,-1.29135232087876,
-1.28024526635582,-1.26930938300003,-1.2531824727869,-1.19460878790403,
-1.1380281402389,-1.1269544534409,-1.12047486614745,-1.11412652524273,-1.10368073934768,
-1.09054784637145,-1.05984279983027,-0.987904838680315,-0.97157369331838,
-0.961702447578007,-0.950851274858951,-0.93517204277001,-0.91687745879115,
-0.878744533463983,-0.818394879822658,-0.807684334784296,-0.801282660555561,
-0.794863494461416,-0.784079266325534,-0.736541400956773,-0.670341716572371,
-0.662034792948836),.UNSPECIFIED.);
#54=B_SPLINE_CURVE_WITH_KNOTS('',3,(#3253,#3254,#3255,#3256,#3257,#3258,
#3259,#3260,#3261,#3262,#3263,#3264,#3265,#3266,#3267,#3268,#3269,#3270,
#3271,#3272,#3273,#3274,#3275,#3276,#3277,#3278,#3279,#3280,#3281,#3282,
#3283,#3284,#3285,#3286,#3287,#3288,#3289,#3290,#3291,#3292,#3293,#3294,
#3295,#3296,#3297,#3298,#3299,#3300,#3301,#3302,#3303,#3304,#3305,#3306,
#3307,#3308,#3309,#3310,#3311,#3312,#3313,#3314,#3315,#3316,#3317,#3318,
#3319,#3320,#3321,#3322,#3323,#3324,#3325,#3326,#3327,#3328,#3329,#3330,
#3331,#3332,#3333,#3334,#3335,#3336,#3337,#3338,#3339,#3340,#3341,#3342,
#3343,#3344,#3345,#3346,#3347,#3348,#3349,#3350,#3351,#3352,#3353,#3354,
#3355,#3356,#3357,#3358,#3359,#3360,#3361,#3362,#3363,#3364,#3365,#3366,
#3367,#3368,#3369,#3370,#3371,#3372,#3373,#3374,#3375,#3376,#3377,#3378,
#3379,#3380,#3381,#3382,#3383,#3384,#3385,#3386,#3387,#3388,#3389,#3390,
#3391,#3392,#3393,#3394,#3395,#3396,#3397,#3398,#3399,#3400,#3401,#3402,
#3403,#3404,#3405,#3406,#3407,#3408,#3409,#3410,#3411,#3412,#3413,#3414,
#3415,#3416,#3417,#3418,#3419,#3420,#3421,#3422,#3423,#3424,#3425,#3426,
#3427,#3428,#3429,#3430),.UNSPECIFIED.,.F.,.F.,(4,2,2,2,2,2,2,2,2,2,2,2,
2,2,2,2,2,2,2,2,2,2,2,2,2,2,2,2,2,2,2,2,2,2,2,2,2,2,2,2,2,2,2,2,2,2,2,2,
2,2,2,2,2,2,2,2,2,2,2,2,2,2,2,2,2,2,2,2,2,2,2,2,2,2,2,2,2,2,2,2,2,2,2,2,
2,2,2,2,4),(-3.39903664743057,-3.36922949716159,-3.35907016472613,-3.35278253154188,
-3.34624369901061,-3.33485442673028,-3.28197372785829,-3.21962138318406,
-3.20385669522807,-3.19299651463027,-3.18314892719787,-3.16693426233528,
-3.09411928565292,-3.06379295586029,-3.05075490729438,-3.04036761404322,
-3.03403448904572,-3.02755269167242,-3.01644165787922,-2.96108432315832,
-2.90045754548251,-2.88480463462061,-2.87396358925092,-2.86409652646892,
-2.84776137026498,-2.77584054112386,-2.74509775457727,-2.73195758796762,
-2.72150990534484,-2.7151645690845,-2.70869698255478,-2.69765504586794,
-2.64078732021274,-2.58206388998048,-2.56617714578574,-2.55529582090197,
-2.54415894673355,-2.5268644748549,-2.47932311619691,-2.43272354330095,
-2.41636129984253,-2.40408963303116,-2.39737281942042,-2.3912707165942,
-2.38177347981764,-2.3481760968759,-2.29029580853658,-2.26789630846598,
-2.24972523294346,-2.23842305127295,-2.22776912237473,-2.21260571020353,
-2.16248563807822,-2.11434921241432,-2.09773424810769,-2.08532581046688,
-2.07858164020483,-2.07249240692179,-2.06307048429426,-2.03081936839389,
-1.97559527017083,-1.9405180689747,-1.92767654069113,-1.91700738834137,
-1.90573216466856,-1.88770565492006,-1.86555124005718,-1.80919432109441,
-1.77362524087514,-1.76405303472052,-1.75793753584351,-1.75124596386142,
-1.73910228569866,-1.7229773003303,-1.67776166540375,-1.62843024292933,
-1.61114088252377,-1.60000448577954,-1.58912150796141,-1.57322857549015,
-1.51442843009721,-1.45758331869308,-1.44653422535539,-1.44006485634313,
-1.43371982394962,-1.42327628194991,-1.41014495002222,-1.37943716657379,
-1.36964803891745),.UNSPECIFIED.);
#55=B_SPLINE_CURVE_WITH_KNOTS('',3,(#3432,#3433,#3434,#3435,#3436,#3437,
#3438,#3439,#3440,#3441,#3442,#3443,#3444,#3445,#3446,#3447,#3448,#3449,
#3450,#3451,#3452,#3453,#3454,#3455,#3456,#3457,#3458,#3459,#3460,#3461,
#3462,#3463,#3464,#3465,#3466,#3467,#3468,#3469,#3470,#3471,#3472,#3473,
#3474,#3475,#3476,#3477,#3478,#3479,#3480,#3481,#3482,#3483,#3484,#3485,
#3486,#3487,#3488,#3489),.UNSPECIFIED.,.F.,.F.,(4,2,2,2,2,2,2,2,2,2,2,2,
2,2,2,2,2,2,2,2,2,2,2,2,2,2,2,2,4),(-0.662034792948836,-0.653334308078723,
-0.642240876193188,-0.631298979652384,-0.615126147845094,-0.558854990744257,
-0.499712483035183,-0.488868934274772,-0.482436762461079,-0.476041922576952,
-0.465376724725386,-0.451872151391653,-0.419622602034269,-0.350862918782535,
-0.334130010188623,-0.32308782579176,-0.312102313169959,-0.295681606448517,
-0.240217946299654,-0.180688818274785,-0.169885524452651,-0.163462444525048,
-0.157060866801764,-0.146361255485615,-0.100197793993894,-0.0337464379318014,
-0.0164341699529654,-0.00773988275201024,-0.000934617407798161),
 .UNSPECIFIED.);
#56=B_SPLINE_CURVE_WITH_KNOTS('',3,(#3490,#3491,#3492,#3493,#3494,#3495,
#3496,#3497,#3498,#3499,#3500,#3501,#3502,#3503,#3504,#3505,#3506,#3507,
#3508,#3509,#3510,#3511,#3512,#3513,#3514,#3515,#3516,#3517,#3518,#3519,
#3520,#3521,#3522,#3523,#3524,#3525,#3526,#3527,#3528,#3529,#3530,#3531,
#3532,#3533,#3534,#3535,#3536,#3537,#3538,#3539,#3540,#3541,#3542,#3543,
#3544,#3545,#3546,#3547,#3548,#3549,#3550,#3551,#3552,#3553,#3554,#3555,
#3556,#3557,#3558,#3559,#3560,#3561,#3562,#3563,#3564,#3565,#3566,#3567,
#3568,#3569,#3570,#3571,#3572,#3573,#3574,#3575,#3576,#3577,#3578,#3579,
#3580,#3581,#3582,#3583,#3584,#3585,#3586,#3587,#3588,#3589,#3590,#3591,
#3592,#3593,#3594,#3595,#3596,#3597,#3598,#3599,#3600,#3601,#3602,#3603,
#3604,#3605),.UNSPECIFIED.,.F.,.F.,(4,2,2,2,2,2,2,2,2,2,2,2,2,2,2,2,2,2,
2,2,2,2,2,2,2,2,2,2,2,2,2,2,2,2,2,2,2,2,2,2,2,2,2,2,2,2,2,2,2,2,2,2,2,2,
2,2,2,4),(-4.05961831363024,-4.04941971591903,-4.03366125775226,-3.96879386302192,
-3.91912535132764,-3.90901225897516,-3.90272988290464,-3.89616876119144,
-3.88468934003338,-3.84670355831125,-3.79478196793746,-3.77341541293937,
-3.75585035176678,-3.74465509405993,-3.73392111606877,-3.71831307817265,
-3.6412008837597,-3.6127881932907,-3.60022959663044,-3.59012613039812,-3.58384522078611,
-3.57728091650738,-3.56578654616062,-3.51421207719407,-3.4715275359027,
-3.45210730791552,-3.43572344931073,-3.42474592312127,-3.41369891317093,
-3.39693282190431,-3.32842069065548,-3.29601708814427,-3.28247633892739,
-3.27179131459786,-3.26539331721021,-3.25896832690889,-3.24815289206938,
-3.18881927595919,-3.15025592705087,-3.13185057655645,-3.11609959348404,
-3.10523330941385,-3.09536970008021,-3.0791020399664,-3.00662330877959,
-2.97614498858093,-2.9630661899283,-2.95265273570601,-2.94631003919231,
-2.93982389023707,-2.9287122749783,-2.87320510605371,-2.81281539045674,
-2.79711436097577,-2.78625657025535,-2.77638416514615,-2.76006237935573,
-2.69113860699559),.UNSPECIFIED.);
#57=B_SPLINE_CURVE_WITH_KNOTS('',3,(#3611,#3612,#3613,#3614,#3615,#3616,
#3617,#3618,#3619,#3620,#3621,#3622,#3623,#3624,#3625,#3626,#3627,#3628,
#3629,#3630,#3631,#3632,#3633,#3634,#3635,#3636,#3637,#3638,#3639,#3640,
#3641,#3642,#3643,#3644,#3645,#3646,#3647,#3648,#3649,#3650,#3651,#3652,
#3653,#3654,#3655,#3656,#3657,#3658,#3659,#3660,#3661,#3662,#3663,#3664,
#3665,#3666,#3667,#3668,#3669,#3670,#3671,#3672,#3673,#3674,#3675,#3676,
#3677,#3678,#3679,#3680,#3681,#3682,#3683,#3684,#3685,#3686,#3687,#3688,
#3689,#3690,#3691,#3692,#3693,#3694,#3695,#3696,#3697,#3698,#3699,#3700,
#3701,#3702,#3703,#3704,#3705,#3706,#3707,#3708,#3709,#3710,#3711,#3712,
#3713,#3714,#3715,#3716,#3717,#3718,#3719,#3720,#3721,#3722,#3723,#3724,
#3725,#3726,#3727,#3728),.UNSPECIFIED.,.F.,.F.,(4,2,2,2,2,2,2,2,2,2,2,2,
2,2,2,2,2,2,2,2,2,2,2,2,2,2,2,2,2,2,2,2,2,2,2,2,2,2,2,2,2,2,2,2,2,2,2,2,
2,2,2,2,2,2,2,2,2,2,4),(-1.36981720180546,-1.3681188713628,-1.35725933449787,
-1.34150327593904,-1.32308317578451,-1.28445166156793,-1.22516009572961,
-1.21433640455159,-1.2079134779239,-1.20152601902886,-1.190874523418,-1.17738952808723,
-1.14520749098011,-1.07630348163935,-1.05959482152721,-1.04856560236975,
-1.03759164402872,-1.02118730242328,-1.00172714162737,-0.958863918280977,
-0.907422055019664,-0.895958161473722,-0.889403779861678,-0.88312663373266,
-0.873022947901647,-0.823002531995589,-0.758255589547942,-0.741127825549499,
-0.730021179212323,-0.719114203482184,-0.703086216509602,-0.640850055396504,
-0.588556123135333,-0.577047491753894,-0.570483825607396,-0.564212954139896,
-0.554142194544246,-0.54163678578329,-0.513418231789095,-0.435885961905594,
-0.420350257017512,-0.409635435298454,-0.398435739804043,-0.380811447536338,
-0.359338444274976,-0.306848831696698,-0.266233271860153,-0.256517046568699,
-0.250925382457069,-0.244473536378757,-0.233510144547139,-0.219488471898311,
-0.184965325355446,-0.119927069565731,-0.103025005849182,-0.0919601728866959,
-0.0810182857079528,-0.0647931581572279,-0.000906520888964826),
 .UNSPECIFIED.);
#58=B_SPLINE_CURVE_WITH_KNOTS('',3,(#3729,#3730,#3731,#3732,#3733,#3734,
#3735,#3736,#3737,#3738,#3739,#3740,#3741,#3742,#3743,#3744,#3745,#3746,
#3747,#3748,#3749,#3750,#3751,#3752,#3753,#3754,#3755,#3756,#3757,#3758,
#3759,#3760,#3761,#3762,#3763,#3764,#3765,#3766,#3767,#3768,#3769,#3770,
#3771,#3772,#3773,#3774,#3775,#3776,#3777,#3778,#3779,#3780,#3781,#3782,
#3783,#3784),.UNSPECIFIED.,.F.,.F.,(4,2,2,2,2,2,2,2,2,2,2,2,2,2,2,2,2,2,
2,2,2,2,2,2,2,2,2,4),(-4.05976150379792,-4.01900511118112,-4.00372888568568,
-3.99706579203473,-3.99074157164933,-3.98424909733907,-3.97308615513119,
-3.91656945385962,-3.85725742797153,-3.84157728669245,-3.83073156957618,
-3.82086928707462,-3.80456378366424,-3.73242006563606,-3.70178160465181,
-3.68866690442563,-3.67823425697505,-3.67189195132403,-3.66542082629823,
-3.65436176824041,-3.59775916499977,-3.53918587468513,-3.5231233860214,
-3.51221123784039,-3.50111365189575,-3.48403034160817,-3.41870744663764,
-3.39903664743057),.UNSPECIFIED.);
#59=B_SPLINE_CURVE_WITH_KNOTS('',3,(#3785,#3786,#3787,#3788,#3789,#3790,
#3791,#3792,#3793,#3794,#3795,#3796,#3797,#3798,#3799,#3800,#3801,#3802,
#3803,#3804,#3805,#3806,#3807,#3808,#3809,#3810,#3811,#3812,#3813,#3814,
#3815,#3816,#3817,#3818,#3819,#3820,#3821,#3822,#3823,#3824,#3825,#3826,
#3827,#3828,#3829,#3830,#3831,#3832,#3833,#3834,#3835,#3836,#3837,#3838,
#3839,#3840,#3841,#3842,#3843,#3844,#3845,#3846,#3847,#3848,#3849,#3850,
#3851,#3852,#3853,#3854,#3855,#3856,#3857,#3858,#3859,#3860,#3861,#3862,
#3863,#3864,#3865,#3866,#3867,#3868,#3869,#3870,#3871,#3872,#3873,#3874,
#3875,#3876,#3877,#3878,#3879,#3880,#3881,#3882,#3883,#3884,#3885,#3886,
#3887,#3888,#3889,#3890,#3891,#3892,#3893,#3894,#3895,#3896,#3897,#3898,
#3899,#3900,#3901,#3902,#3903,#3904,#3905,#3906,#3907,#3908,#3909,#3910,
#3911,#3912,#3913,#3914,#3915,#3916,#3917,#3918,#3919,#3920,#3921,#3922,
#3923,#3924,#3925,#3926,#3927,#3928,#3929,#3930,#3931,#3932,#3933,#3934,
#3935,#3936,#3937,#3938,#3939,#3940,#3941,#3942,#3943,#3944,#3945,#3946,
#3947,#3948,#3949,#3950,#3951,#3952,#3953,#3954,#3955,#3956,#3957,#3958,
#3959,#3960,#3961,#3962,#3963,#3964),.UNSPECIFIED.,.F.,.F.,(4,2,2,2,2,2,
2,2,2,2,2,2,2,2,2,2,2,2,2,2,2,2,2,2,2,2,2,2,2,2,2,2,2,2,2,2,2,2,2,2,2,2,
2,2,2,2,2,2,2,2,2,2,2,2,2,2,2,2,2,2,2,2,2,2,2,2,2,2,2,2,2,2,2,2,2,2,2,2,
2,2,2,2,2,2,2,2,2,2,2,4),(-2.69113860699559,-2.68798641270898,-2.65732048758469,
-2.6441957050177,-2.63375504946037,-2.62740682579674,-2.62092706332233,
-2.60984650514142,-2.55354048871653,-2.49436614744855,-2.47845167620463,
-2.46755708279682,-2.45641033162421,-2.43910649863235,-2.38942595349833,
-2.34444481724778,-2.32835480078381,-2.31622898493564,-2.30953702939491,
-2.30341145852001,-2.29380726516983,-2.25763113264322,-2.20182075057012,
-2.17975829556766,-2.16178098829088,-2.15050742299244,-2.13981979878661,
-2.12693032583511,-2.09136959620799,-2.03000581693164,-2.00345394327482,
-1.99448025809388,-1.98839852765128,-1.98143124757679,-1.96789403242635,
-1.94913114223327,-1.88490277518901,-1.85197717243011,-1.83816279184475,
-1.82755156107063,-1.81577379888628,-1.79512201956957,-1.76828506562415,
-1.72308524164038,-1.6860054757428,-1.67636393420948,-1.6707812387932,-1.66429854220551,
-1.65320306393962,-1.63895485811311,-1.60341497517815,-1.54061867241779,
-1.52334944633781,-1.51220937656063,-1.50131012230862,-1.48536808094627,
-1.42556276183992,-1.36993616332764,-1.35882588238135,-1.35234009620102,
-1.34599709334049,-1.33558250789777,-1.32250316497891,-1.29201938113414,
-1.21962447199833,-1.20335376357977,-1.19348971912112,-1.18262382552945,
-1.16687554439054,-1.10608193557756,-1.05104877082362,-1.03991809875167,
-1.03342803251385,-1.02708841092747,-1.0166910281483,-1.0036408448629,-0.973276175239219,
-0.900621350267408,-0.884385297518919,-0.874526685836425,-0.863654915143497,
-0.847873423334712,-0.787349729372831,-0.7321027352839,-0.720979885217171,
-0.714491338462904,-0.708150183255675,-0.697745635827008,-0.684683444874573,
-0.661711247179129),.UNSPECIFIED.);
#60=B_SPLINE_CURVE_WITH_KNOTS('',3,(#3969,#3970,#3971,#3972,#3973,#3974,
#3975,#3976,#3977,#3978,#3979,#3980,#3981,#3982,#3983,#3984,#3985,#3986,
#3987,#3988,#3989,#3990,#3991,#3992,#3993,#3994,#3995,#3996,#3997,#3998,
#3999,#4000,#4001,#4002,#4003,#4004,#4005,#4006,#4007,#4008,#4009,#4010,
#4011,#4012,#4013,#4014,#4015,#4016,#4017,#4018,#4019,#4020,#4021,#4022,
#4023,#4024,#4025,#4026,#4027,#4028,#4029,#4030,#4031,#4032,#4033,#4034,
#4035,#4036,#4037,#4038,#4039,#4040,#4041,#4042,#4043,#4044,#4045,#4046,
#4047,#4048,#4049,#4050,#4051,#4052,#4053,#4054,#4055,#4056,#4057,#4058,
#4059,#4060,#4061,#4062,#4063,#4064,#4065,#4066,#4067,#4068,#4069,#4070,
#4071,#4072,#4073,#4074,#4075,#4076,#4077,#4078,#4079,#4080,#4081,#4082,
#4083,#4084,#4085,#4086,#4087,#4088,#4089,#4090,#4091,#4092,#4093,#4094,
#4095,#4096,#4097,#4098,#4099,#4100,#4101,#4102,#4103,#4104,#4105,#4106,
#4107,#4108,#4109,#4110,#4111,#4112,#4113,#4114,#4115,#4116,#4117,#4118,
#4119,#4120,#4121,#4122,#4123,#4124,#4125,#4126,#4127,#4128,#4129,#4130,
#4131,#4132,#4133,#4134,#4135,#4136),.UNSPECIFIED.,.F.,.F.,(4,2,2,2,2,2,
2,2,2,2,2,2,2,2,2,2,2,2,2,2,2,2,2,2,2,2,2,2,2,2,2,2,2,2,2,2,2,2,2,2,2,2,
2,2,2,2,2,2,2,2,2,2,2,2,2,2,2,2,2,2,2,2,2,2,2,2,2,2,2,2,2,2,2,2,2,2,2,2,
2,2,2,2,2,4),(-3.39942278040286,-3.36860646077918,-3.30661711098668,-3.29089667379652,
-3.28004385360924,-3.27018829158702,-3.25392549459415,-3.181459301777,-3.15096955861408,
-3.13789115452488,-3.12747989811296,-3.12114181025084,-3.11466542925515,
-3.10358134826762,-3.04744846003736,-2.9891769177977,-2.97277475043909,
-2.96180178103899,-2.95077308870415,-2.93406452113314,-2.86510808270885,
-2.83292156853096,-2.8194349560482,-2.80878352066393,-2.80239642731346,
-2.79597398138058,-2.7851516586564,-2.72591483166686,-2.68729596296793,
-2.66888070043975,-2.65312665475517,-2.64226783058902,-2.63241769664277,
-2.61618983721396,-2.54346049584816,-2.51309087869975,-2.50004184354062,
-2.48964788974661,-2.48331317394372,-2.47683243672944,-2.46572775980563,
-2.4101427310699,-2.34974837996218,-2.33408374219892,-2.32324021701081,
-2.31337449294839,-2.29705021717626,-2.2250362562185,-2.19433343314705,
-2.1812026904133,-2.17076041568238,-2.16441592584437,-2.15794655445302,
-2.14689714833195,-2.09012809837676,-2.03094814088529,-2.01522472499628,
-2.00447907371533,-1.99332736545466,-1.9759559845059,-1.92496161228227,
-1.86225808614346,-1.85182627721601,-1.8454838684314,-1.83901197204939,
-1.82795048098781,-1.8137582331815,-1.7784616874252,-1.71524122589339,-1.69800344107717,
-1.68687659084232,-1.67598615600202,-1.66005090821033,-1.60022607650516,
-1.54460087284301,-1.53349452438244,-1.52701335837661,-1.52067855549214,
-1.51028531743975,-1.49723902395652,-1.46687822163521,-1.39419612160138,
-1.37796907845977,-1.36981720180546),.UNSPECIFIED.);
#61=B_SPLINE_CURVE_WITH_KNOTS('',3,(#4138,#4139,#4140,#4141,#4142,#4143,
#4144,#4145,#4146,#4147,#4148,#4149,#4150,#4151,#4152,#4153,#4154,#4155,
#4156,#4157,#4158,#4159,#4160,#4161,#4162,#4163,#4164,#4165,#4166,#4167,
#4168,#4169,#4170,#4171,#4172,#4173,#4174,#4175,#4176,#4177,#4178,#4179,
#4180,#4181,#4182,#4183,#4184,#4185,#4186,#4187,#4188,#4189,#4190,#4191),
 .UNSPECIFIED.,.F.,.F.,(4,2,2,2,2,2,2,2,2,2,2,2,2,2,2,2,2,2,2,2,2,2,2,2,
2,2,4),(-0.661711247179129,-0.654270438906596,-0.581717180746494,-0.565466795777757,
-0.555605724287503,-0.544735994000254,-0.528967360918269,-0.468992020429739,
-0.413129166744064,-0.402025820592833,-0.395541194624966,-0.389196450444212,
-0.378774569908438,-0.365683181090854,-0.335151734656965,-0.262850577953034,
-0.246565590468353,-0.236698783708754,-0.225834321032208,-0.210097398454042,
-0.150731747581798,-0.0941220267533644,-0.0830532554658109,-0.0765756499766033,
-0.0702245991095249,-0.0597719941297826,-0.000906261498553894),
 .UNSPECIFIED.);
#62=B_SPLINE_CURVE_WITH_KNOTS('',3,(#4192,#4193,#4194,#4195,#4196,#4197,
#4198,#4199,#4200,#4201,#4202,#4203,#4204,#4205,#4206,#4207,#4208,#4209,
#4210,#4211,#4212,#4213,#4214,#4215,#4216,#4217,#4218,#4219,#4220,#4221,
#4222,#4223,#4224,#4225,#4226,#4227,#4228,#4229,#4230,#4231,#4232,#4233,
#4234,#4235,#4236,#4237,#4238,#4239,#4240,#4241,#4242,#4243,#4244,#4245,
#4246,#4247,#4248,#4249,#4250,#4251,#4252,#4253,#4254,#4255,#4256,#4257,
#4258,#4259,#4260,#4261,#4262,#4263,#4264,#4265,#4266,#4267,#4268,#4269,
#4270,#4271,#4272,#4273,#4274,#4275,#4276,#4277,#4278,#4279,#4280,#4281,
#4282,#4283,#4284,#4285,#4286,#4287,#4288,#4289,#4290,#4291,#4292,#4293,
#4294,#4295,#4296,#4297,#4298,#4299,#4300,#4301,#4302,#4303,#4304,#4305,
#4306,#4307),.UNSPECIFIED.,.F.,.F.,(4,2,2,2,2,2,2,2,2,2,2,2,2,2,2,2,2,2,
2,2,2,2,2,2,2,2,2,2,2,2,2,2,2,2,2,2,2,2,2,2,2,2,2,2,2,2,2,2,2,2,2,2,2,2,
2,2,2,4),(-4.06006106737699,-4.01750335279925,-3.99679661475175,-3.98597230434252,
-3.97513721085419,-3.96524400160451,-3.94878727173729,-3.87701512354494,
-3.84635395252591,-3.83323120657681,-3.82279217357101,-3.81644494367554,
-3.80996619369454,-3.79888739309778,-3.74258921628807,-3.68298461951677,
-3.66727133834649,-3.65641272700456,-3.64654443939987,-3.6302411468607,
-3.55805664022011,-3.52745122944711,-3.51434211880632,-3.5039111418175,
-3.49756553738962,-3.49108488766042,-3.47999686921938,-3.42389233184436,
-3.38364093332244,-3.36480936582705,-3.34879168219368,-3.33788008897764,
-3.32675855470048,-3.30958460206247,-3.2453173690025,-3.19512318986539,
-3.18488631148219,-3.17857952331764,-3.17205112158684,-3.16073081605242,
-3.09153482140168,-3.04526653381446,-3.02954790578215,-3.01868825256711,
-3.00882070279101,-2.99252267151132,-2.9202959297447,-2.88970923791968,
-2.87660462294926,-2.86617626172096,-2.85983112000475,-2.85334971532542,
-2.84225834448629,-2.78622659086253,-2.72621098959534,-2.71057131022136,
-2.69972510548116,-2.69144328541572),.UNSPECIFIED.);
#63=B_SPLINE_CURVE_WITH_KNOTS('',3,(#4313,#4314,#4315,#4316,#4317,#4318,
#4319,#4320,#4321,#4322,#4323,#4324,#4325,#4326,#4327,#4328,#4329,#4330,
#4331,#4332,#4333,#4334,#4335,#4336,#4337,#4338,#4339,#4340,#4341,#4342,
#4343,#4344,#4345,#4346,#4347,#4348,#4349,#4350,#4351,#4352,#4353,#4354,
#4355,#4356,#4357,#4358,#4359,#4360,#4361,#4362,#4363,#4364,#4365,#4366,
#4367,#4368,#4369,#4370,#4371,#4372,#4373,#4374,#4375,#4376,#4377,#4378,
#4379,#4380,#4381,#4382,#4383,#4384,#4385,#4386,#4387,#4388,#4389,#4390,
#4391,#4392,#4393,#4394,#4395,#4396,#4397,#4398,#4399,#4400,#4401,#4402,
#4403,#4404,#4405,#4406,#4407,#4408,#4409,#4410,#4411,#4412,#4413,#4414,
#4415,#4416,#4417,#4418,#4419,#4420,#4421,#4422,#4423,#4424,#4425,#4426,
#4427,#4428,#4429,#4430,#4431,#4432,#4433,#4434,#4435,#4436,#4437,#4438,
#4439,#4440,#4441,#4442),.UNSPECIFIED.,.F.,.F.,(4,2,2,2,2,2,2,2,2,2,2,2,
2,2,2,2,2,2,2,2,2,2,2,2,2,2,2,2,2,2,2,2,2,2,2,2,2,2,2,2,2,2,2,2,2,2,2,2,
2,2,2,2,2,2,2,2,2,2,2,2,2,2,2,2,4),(-1.36945801245357,-1.31142024483846,
-1.30064223896015,-1.29422830883802,-1.28783078031624,-1.27713254417671,
-1.26356810040954,-1.23105027367383,-1.16279279380772,-1.14600723349723,
-1.13496307828971,-1.12400073344613,-1.10766562054501,-1.08831820292282,
-1.04593815898459,-0.99387169077095,-0.982330811192836,-0.975760293128391,
-0.969493552026457,-0.959445472599736,-0.946978091374135,-0.918907391364276,
-0.841015863050523,-0.825531436441148,-0.814824528981982,-0.803610376227102,
-0.785912074939119,-0.764314985243115,-0.711154153356489,-0.671449111270555,
-0.661742398995181,-0.656152076178251,-0.649696954949905,-0.638719033331854,
-0.624672506223117,-0.590039617324983,-0.525679578965086,-0.508519715582898,
-0.497406577252715,-0.486503466719564,-0.470500512594571,-0.451687123957076,
-0.411505667934827,-0.35516082373592,-0.344081429726595,-0.337605473764751,
-0.331265281005552,-0.320847026760153,-0.307758819139739,-0.277229206573372,
-0.204899998177409,-0.18862312446602,-0.178764301512738,-0.167911687930887,
-0.152199756021093,-0.13385028428509,-0.0954945839976622,-0.078738321637529,
-0.0782343598820795,-0.0540345406664802,-0.0311753977701198,-0.0226064955066162,
-0.0166883237025578,-0.0110430614363735,-0.000905562748328462),
 .UNSPECIFIED.);
#64=B_SPLINE_CURVE_WITH_KNOTS('',3,(#4443,#4444,#4445,#4446,#4447,#4448,
#4449,#4450,#4451,#4452,#4453,#4454,#4455,#4456,#4457,#4458,#4459,#4460,
#4461,#4462,#4463,#4464,#4465,#4466,#4467,#4468,#4469,#4470,#4471,#4472,
#4473,#4474,#4475,#4476,#4477,#4478,#4479,#4480,#4481,#4482,#4483,#4484,
#4485,#4486,#4487,#4488,#4489,#4490,#4491,#4492,#4493,#4494,#4495,#4496,
#4497,#4498,#4499,#4500),.UNSPECIFIED.,.F.,.F.,(4,2,2,2,2,2,2,2,2,2,2,2,
2,2,2,2,2,2,2,2,2,2,2,2,2,2,2,2,4),(-4.06049499041426,-4.00144584921642,
-3.96288024512554,-3.94447915811091,-3.92873425089659,-3.91787742515527,
-3.90802638356343,-3.89179053725541,-3.8191300166447,-3.78873192773811,
-3.77567617873277,-3.76527839089358,-3.75894312369514,-3.75246376712777,
-3.74136473286814,-3.68562532702502,-3.6451432106023,-3.62625800758028,
-3.61020961699309,-3.5992997388205,-3.58819870002538,-3.5710979320657,-3.50597092402198,
-3.45651578954256,-3.44626001988021,-3.4399531399171,-3.43343884263639,
-3.42217007433208,-3.39942278040286),.UNSPECIFIED.);
#65=B_SPLINE_CURVE_WITH_KNOTS('',3,(#4501,#4502,#4503,#4504,#4505,#4506,
#4507,#4508,#4509,#4510,#4511,#4512,#4513,#4514,#4515,#4516,#4517,#4518,
#4519,#4520,#4521,#4522,#4523,#4524,#4525,#4526,#4527,#4528,#4529,#4530,
#4531,#4532,#4533,#4534,#4535,#4536,#4537,#4538,#4539,#4540,#4541,#4542,
#4543,#4544,#4545,#4546,#4547,#4548,#4549,#4550,#4551,#4552,#4553,#4554,
#4555,#4556,#4557,#4558,#4559,#4560,#4561,#4562,#4563,#4564,#4565,#4566,
#4567,#4568,#4569,#4570,#4571,#4572,#4573,#4574,#4575,#4576,#4577,#4578,
#4579,#4580,#4581,#4582,#4583,#4584,#4585,#4586,#4587,#4588,#4589,#4590,
#4591,#4592,#4593,#4594,#4595,#4596,#4597,#4598,#4599,#4600,#4601,#4602,
#4603,#4604,#4605,#4606,#4607,#4608,#4609,#4610,#4611,#4612,#4613,#4614,
#4615,#4616,#4617,#4618,#4619,#4620,#4621,#4622,#4623,#4624,#4625,#4626,
#4627,#4628,#4629,#4630,#4631,#4632,#4633,#4634,#4635,#4636,#4637,#4638,
#4639,#4640,#4641,#4642,#4643,#4644,#4645,#4646,#4647,#4648,#4649,#4650,
#4651,#4652,#4653,#4654,#4655,#4656,#4657,#4658,#4659,#4660,#4661,#4662,
#4663,#4664,#4665,#4666,#4667,#4668,#4669,#4670),.UNSPECIFIED.,.F.,.F.,
(4,2,2,2,2,2,2,2,2,2,2,2,2,2,2,2,2,2,2,2,2,2,2,2,2,2,2,2,2,2,2,2,2,2,2,
2,2,2,2,2,2,2,2,2,2,2,2,2,2,2,2,2,2,2,2,2,2,2,2,2,2,2,2,2,2,2,2,2,2,2,2,
2,2,2,2,2,2,2,2,2,2,2,2,2,4),(-2.69144328541572,-2.68984354191311,-2.6734590655946,
-2.60188261593871,-2.57099026285687,-2.5578110604289,-2.54733864671877,
-2.54098458216743,-2.53451345177249,-2.52347202960527,-2.46655502948031,
-2.42675887634366,-2.40804080870372,-2.39209402188225,-2.38119471500536,
-2.37005703621845,-2.35279703322566,-2.2897867238274,-2.25434268394012,
-2.24011463291027,-2.22903182543274,-2.22255217296172,-2.21696857426285,
-2.20731965679741,-2.16998655160728,-2.12990077757589,-2.08645651695713,
-2.07171127318128,-2.06100766230234,-2.04952231521939,-2.0304225382796,
-1.95320558070817,-1.9182698872082,-1.90872424528372,-1.90260931108544,
-1.8958978379517,-1.88367357207352,-1.8674042989991,-1.82136134023027,-1.77321295786483,
-1.7558882821052,-1.7447380060636,-1.73384682361741,-1.71795030763093,-1.6592432013438,
-1.60230439078201,-1.59125824821918,-1.58478572683239,-1.57843146322911,
-1.56796088219368,-1.554786700059,-1.52391432331564,-1.45235070424489,-1.43596962916131,
-1.42608783923466,-1.41523947059035,-1.3995930622834,-1.33873655493508,
-1.28352895692786,-1.27240522765314,-1.26591665706296,-1.25957596371069,
-1.24917292186661,-1.2361131060364,-1.2057089125561,-1.13314178524207,-1.11689425384144,
-1.10703391210559,-1.09616422354748,-1.08039406338827,-1.01840076745309,
-0.96491192182675,-0.953617134107769,-0.947093377713306,-0.940781185641492,
-0.930520787210808,-0.880910983917029,-0.816043382298155,-0.798919574871243,
-0.787806083072503,-0.776884739936868,-0.760819508783053,-0.741910938442555,
-0.701360367414784,-0.662002611929399),.UNSPECIFIED.);
#66=B_SPLINE_CURVE_WITH_KNOTS('',3,(#4675,#4676,#4677,#4678,#4679,#4680,
#4681,#4682,#4683,#4684,#4685,#4686,#4687,#4688,#4689,#4690,#4691,#4692,
#4693,#4694,#4695,#4696,#4697,#4698,#4699,#4700,#4701,#4702,#4703,#4704,
#4705,#4706,#4707,#4708,#4709,#4710,#4711,#4712,#4713,#4714,#4715,#4716,
#4717,#4718,#4719,#4720,#4721,#4722,#4723,#4724,#4725,#4726,#4727,#4728,
#4729,#4730,#4731,#4732,#4733,#4734,#4735,#4736,#4737,#4738,#4739,#4740,
#4741,#4742,#4743,#4744,#4745,#4746,#4747,#4748,#4749,#4750,#4751,#4752,
#4753,#4754,#4755,#4756,#4757,#4758,#4759,#4760,#4761,#4762,#4763,#4764,
#4765,#4766,#4767,#4768,#4769,#4770,#4771,#4772,#4773,#4774,#4775,#4776,
#4777,#4778,#4779,#4780,#4781,#4782,#4783,#4784,#4785,#4786,#4787,#4788,
#4789,#4790,#4791,#4792,#4793,#4794,#4795,#4796,#4797,#4798,#4799,#4800,
#4801,#4802,#4803,#4804,#4805,#4806,#4807,#4808,#4809,#4810,#4811,#4812,
#4813,#4814,#4815,#4816,#4817,#4818,#4819,#4820,#4821,#4822,#4823,#4824,
#4825,#4826,#4827,#4828,#4829,#4830,#4831,#4832,#4833,#4834,#4835,#4836,
#4837,#4838,#4839,#4840,#4841,#4842,#4843,#4844,#4845,#4846,#4847,#4848,
#4849,#4850,#4851,#4852,#4853,#4854),.UNSPECIFIED.,.F.,.F.,(4,2,2,2,2,2,
2,2,2,2,2,2,2,2,2,2,2,2,2,2,2,2,2,2,2,2,2,2,2,2,2,2,2,2,2,2,2,2,2,2,2,2,
2,2,2,2,2,2,2,2,2,2,2,2,2,2,2,2,2,2,2,2,2,2,2,2,2,2,2,2,2,2,2,2,2,2,2,2,
2,2,2,2,2,2,2,2,2,2,2,4),(-3.39931823127231,-3.39333264987127,-3.37756827591752,
-3.36670620862625,-3.35685556675115,-3.34063265312326,-3.26783032142072,
-3.23748196806637,-3.22443722634335,-3.21404537554358,-3.20771043435399,
-3.20122812368755,-3.19011814782567,-3.13464457245426,-3.07398882591856,
-3.05838385281095,-3.0475495776618,-3.03767179376624,-3.02127810996635,
-2.94975835780466,-2.91881082611094,-2.90561973271878,-2.89514150456081,
-2.88878926325972,-2.88232696973456,-2.87131519171508,-2.81399875021888,
-2.75560750759241,-2.73973186427994,-2.72885060565196,-2.71770773700242,
-2.70039086481708,-2.63847598162576,-2.60232605128182,-2.58794665558805,
-2.57677834537134,-2.57028388514838,-2.56395871948222,-2.5536158045003,
-2.4901750847304,-2.43966620504835,-2.42235596467229,-2.41121441925878,
-2.40045844217865,-2.38468223245109,-2.30871712696938,-2.27978735843464,
-2.26709804253308,-2.25691762101437,-2.2506248533669,-2.24408947435361,
-2.23272172362556,-2.16630689634555,-2.12634380276431,-2.10600922698734,
-2.09429691446114,-2.08368046666383,-2.06976763500726,-2.03638687518432,
-2.03024396124456,-1.98802964114676,-1.94725005922582,-1.93753186880774,
-1.93193951805665,-1.92548737399093,-1.91452445214204,-1.90050406163128,
-1.86598932803968,-1.80142067547124,-1.7842765179594,-1.77316607936646,
-1.76226027148026,-1.74624324958776,-1.72740752156719,-1.6871371509107,
-1.63094392166677,-1.61985703293382,-1.61337941640967,-1.60704032057634,
-1.59662804178187,-1.58355005322157,-1.55306269092771,-1.4806391556512,
-1.46437433870505,-1.45451727871944,-1.44366240155752,-1.42793847442011,
-1.40957012536622,-1.37114240909329,-1.36945801245357),.UNSPECIFIED.);
#67=B_SPLINE_CURVE_WITH_KNOTS('',3,(#4856,#4857,#4858,#4859,#4860,#4861,
#4862,#4863,#4864,#4865,#4866,#4867,#4868,#4869,#4870,#4871,#4872,#4873,
#4874,#4875,#4876,#4877,#4878,#4879,#4880,#4881,#4882,#4883,#4884,#4885,
#4886,#4887,#4888,#4889,#4890,#4891,#4892,#4893,#4894,#4895,#4896,#4897,
#4898,#4899,#4900,#4901,#4902,#4903,#4904,#4905,#4906,#4907,#4908,#4909,
#4910,#4911,#4912,#4913),.UNSPECIFIED.,.F.,.F.,(4,2,2,2,2,2,2,2,2,2,2,2,
2,2,2,2,2,2,2,2,2,2,2,2,2,2,2,2,4),(-0.662002611929399,-0.645673022059062,
-0.634564153273406,-0.628078498344257,-0.621734934376972,-0.611318364231216,
-0.598235837861409,-0.567739945548748,-0.495365854606088,-0.479091350770045,
-0.469226419918645,-0.458360624311453,-0.442614716404333,-0.382164873145699,
-0.326752710107995,-0.315635002362123,-0.309147441075794,-0.302805245738295,
-0.292395906945934,-0.279325698342569,-0.248880459281276,-0.176394415429904,
-0.16013448638823,-0.15027175151832,-0.13940332751517,-0.123643119994858,
-0.061539183838578,-0.0147529766196489,-0.000906767077203394),
 .UNSPECIFIED.);
#68=B_SPLINE_CURVE_WITH_KNOTS('',3,(#4914,#4915,#4916,#4917,#4918,#4919,
#4920,#4921,#4922,#4923,#4924,#4925,#4926,#4927,#4928,#4929,#4930,#4931,
#4932,#4933,#4934,#4935,#4936,#4937,#4938,#4939,#4940,#4941,#4942,#4943,
#4944,#4945,#4946,#4947,#4948,#4949,#4950,#4951,#4952,#4953,#4954,#4955,
#4956,#4957,#4958,#4959,#4960,#4961,#4962,#4963,#4964,#4965,#4966,#4967,
#4968,#4969,#4970,#4971,#4972,#4973,#4974,#4975,#4976,#4977,#4978,#4979,
#4980,#4981,#4982,#4983,#4984,#4985,#4986,#4987,#4988,#4989,#4990,#4991,
#4992,#4993,#4994,#4995,#4996,#4997,#4998,#4999,#5000,#5001,#5002,#5003,
#5004,#5005,#5006,#5007,#5008,#5009,#5010,#5011,#5012,#5013,#5014,#5015,
#5016,#5017,#5018,#5019,#5020,#5021,#5022,#5023,#5024,#5025,#5026,#5027,
#5028,#5029,#5030,#5031,#5032,#5033,#5034,#5035,#5036,#5037,#5038,#5039,
#5040,#5041,#5042,#5043,#5044,#5045,#5046,#5047,#5048,#5049,#5050,#5051,
#5052,#5053,#5054,#5055,#5056,#5057,#5058),.UNSPECIFIED.,.F.,.F.,(4,3,3,
3,3,3,3,3,3,3,3,3,3,3,3,3,3,3,3,3,3,3,3,3,3,3,3,3,3,3,3,3,3,3,3,3,3,3,3,
3,3,3,3,3,3,3,3,3,4),(47.1238898038469,47.1578675480998,47.2510868451706,
47.3441829801613,47.4371833640954,47.5301187067581,47.6230208283606,47.7159143623725,
47.8088239284592,47.9018309388297,47.994890928453,48.0880983142331,48.1451634736649,
48.2383827858837,48.3314789359493,48.4244793348657,48.5174146923123,48.6103168285705,
48.7032103770924,48.7961199575261,48.8891269819078,48.9821869853736,49.0753943845935,
49.1324593992301,49.2256787299236,49.3187748986893,49.4117753165029,49.5047106930589,
49.5976128485495,49.6905064164021,49.7834160162398,49.8764230600177,49.9694830829029,
50.0626905013858,50.1197553247952,50.2129745435564,50.3060706001924,50.3990709058328,
50.4920061706172,50.5849082146287,50.6778016714316,50.7707111607865,50.8637180956196,
50.95677801027,51.0499853227089,51.1070512503604,51.2002688732808,51.293351331344,
51.3612711115601),.UNSPECIFIED.);
#69=B_SPLINE_CURVE_WITH_KNOTS('',3,(#5064,#5065,#5066,#5067,#5068,#5069,
#5070,#5071,#5072,#5073,#5074,#5075,#5076,#5077,#5078,#5079,#5080,#5081,
#5082,#5083,#5084,#5085,#5086,#5087,#5088,#5089,#5090,#5091,#5092,#5093,
#5094,#5095,#5096,#5097,#5098,#5099,#5100,#5101,#5102,#5103,#5104,#5105,
#5106,#5107,#5108,#5109,#5110,#5111,#5112,#5113,#5114,#5115,#5116,#5117,
#5118,#5119,#5120,#5121,#5122,#5123,#5124,#5125,#5126,#5127,#5128,#5129,
#5130,#5131,#5132,#5133,#5134,#5135,#5136,#5137,#5138,#5139,#5140,#5141,
#5142,#5143,#5144,#5145,#5146,#5147,#5148,#5149,#5150,#5151,#5152,#5153,
#5154,#5155,#5156,#5157,#5158,#5159,#5160,#5161,#5162,#5163,#5164,#5165,
#5166,#5167,#5168,#5169,#5170,#5171,#5172,#5173,#5174,#5175,#5176,#5177,
#5178,#5179,#5180,#5181,#5182,#5183,#5184,#5185,#5186,#5187,#5188,#5189,
#5190,#5191,#5192,#5193,#5194,#5195,#5196,#5197,#5198,#5199,#5200,#5201,
#5202,#5203,#5204,#5205),.UNSPECIFIED.,.F.,.F.,(4,3,3,3,3,3,3,3,3,3,3,3,
3,3,3,3,3,3,3,3,3,3,3,3,3,3,3,3,3,3,3,3,3,3,3,3,3,3,3,3,3,3,3,3,3,3,3,4),
(53.4070751113264,53.5154608823167,53.6249212271248,53.7303453258545,53.8235779004443,
53.9166872770643,54.009700849372,54.1026492469518,54.1955643359709,54.2884707342843,
54.3813930458559,54.474412543289,54.5674848923327,54.6607043142074,54.7176412514196,
54.8108646662176,54.903965072386,54.9969698728911,55.0899098282812,55.1828166815042,
55.2757150592943,55.3686295746718,55.4616416636342,55.5547068117602,55.6479194305051,
55.7049371769848,55.7980868069411,55.8911130729797,55.9840434820572,56.076908981525,
56.1697413679859,56.2625653599032,56.3554056621105,56.448344254422,56.5413362031023,
56.6344768169055,56.6922331025499,56.7855972844833,56.8788375378924,56.9744559017533,
57.0675295291053,57.1605689969723,57.2535987650433,57.3511451859774,57.4442771053405,
57.537462070741,57.630767641988,57.6437844487799),.UNSPECIFIED.);
#70=B_SPLINE_CURVE_WITH_KNOTS('',3,(#5206,#5207,#5208,#5209,#5210,#5211,
#5212,#5213,#5214,#5215,#5216,#5217,#5218,#5219,#5220,#5221,#5222,#5223,
#5224,#5225,#5226,#5227,#5228,#5229,#5230,#5231,#5232,#5233,#5234,#5235,
#5236,#5237,#5238,#5239,#5240,#5241,#5242,#5243,#5244,#5245,#5246,#5247,
#5248,#5249,#5250,#5251,#5252,#5253,#5254,#5255,#5256,#5257,#5258,#5259,
#5260,#5261,#5262,#5263),.UNSPECIFIED.,.F.,.F.,(4,2,2,2,2,2,2,2,2,2,2,2,
2,2,2,2,2,2,2,2,2,2,2,2,2,2,2,2,4),(-4.06067588059912,-4.04069247019934,
-4.02617376395736,-4.01534753129665,-4.00544410492176,-3.99444491625099,
-3.97788641249948,-3.90579227222274,-3.87542989373594,-3.86238290113527,
-3.85199059780189,-3.84565758040844,-3.83917673322251,-3.82807514836664,
-3.77232653875084,-3.71201227279839,-3.69636762635081,-3.68552511088964,
-3.6756519977026,-3.65929508343662,-3.58751727900746,-3.55670727552532,
-3.54354924171794,-3.53309014022462,-3.52674073670713,-3.52027266087198,
-3.50923391192641,-3.45227204802997,-3.39931823127231),.UNSPECIFIED.);
#71=B_SPLINE_CURVE_WITH_KNOTS('',3,(#5265,#5266,#5267,#5268,#5269,#5270,
#5271,#5272,#5273,#5274,#5275,#5276,#5277,#5278,#5279,#5280,#5281,#5282,
#5283,#5284,#5285,#5286,#5287,#5288,#5289,#5290,#5291,#5292,#5293,#5294,
#5295,#5296,#5297,#5298,#5299,#5300,#5301,#5302,#5303,#5304,#5305,#5306,
#5307,#5308,#5309,#5310,#5311,#5312,#5313,#5314,#5315,#5316,#5317,#5318,
#5319,#5320,#5321,#5322,#5323,#5324,#5325,#5326,#5327,#5328,#5329,#5330,
#5331),.UNSPECIFIED.,.F.,.F.,(4,3,3,3,3,3,3,3,3,3,3,3,3,3,3,3,3,3,3,3,3,
3,4),(51.3612711115601,51.4542197461849,51.5471285042568,51.6400220262204,
51.7329249334203,51.8259215363716,51.9189651439704,52.0121635352636,52.0943471759255,
52.1875666611415,52.2806629858775,52.3736635608775,52.4665990957627,52.559501410222,
52.6523951374807,52.7453048969597,52.8383120997537,52.9313722815292,53.0245798571289,
53.0816431014906,53.1910683080732,53.299486149192,53.4070751107236),
 .UNSPECIFIED.);
#72=B_SPLINE_CURVE_WITH_KNOTS('',3,(#5332,#5333,#5334,#5335,#5336,#5337,
#5338,#5339,#5340,#5341,#5342,#5343,#5344,#5345,#5346,#5347,#5348,#5349,
#5350,#5351,#5352,#5353,#5354,#5355,#5356,#5357,#5358,#5359,#5360,#5361,
#5362,#5363,#5364,#5365,#5366,#5367,#5368,#5369,#5370,#5371,#5372,#5373,
#5374,#5375,#5376,#5377,#5378,#5379,#5380,#5381,#5382,#5383,#5384,#5385,
#5386,#5387,#5388,#5389,#5390,#5391,#5392,#5393,#5394,#5395,#5396,#5397,
#5398,#5399,#5400,#5401,#5402,#5403,#5404,#5405,#5406,#5407,#5408,#5409,
#5410,#5411,#5412,#5413,#5414,#5415,#5416,#5417,#5418,#5419,#5420,#5421,
#5422,#5423,#5424,#5425,#5426,#5427,#5428,#5429,#5430,#5431,#5432,#5433,
#5434,#5435,#5436,#5437,#5438,#5439,#5440,#5441,#5442,#5443,#5444,#5445,
#5446,#5447,#5448,#5449,#5450,#5451,#5452,#5453,#5454,#5455),
 .UNSPECIFIED.,.F.,.F.,(4,2,2,2,2,2,2,2,2,2,2,2,2,2,2,2,2,2,2,2,2,2,2,2,
2,2,2,2,2,2,2,2,2,2,2,2,2,2,2,2,2,2,2,2,2,2,2,2,2,2,2,2,2,2,2,2,2,2,2,2,
2,4),(1.36958410658186,1.3918117919107,1.40402272121196,1.41456715400893,
1.42790276929566,1.4580462745132,1.50752852260155,1.54885081199774,1.56042948267245,
1.56701194542835,1.57327886096385,1.58331693394143,1.59576779742258,1.62376905121261,
1.70186095396046,1.71732178254663,1.72802773397601,1.73925394769026,1.75700207751367,
1.77867870716166,1.83228882631052,1.87132868801542,1.88102350568051,1.8866132536601,
1.89307842287806,1.90408956688519,1.91819266087862,1.95306614410452,2.01704247204898,
2.03424075566318,2.04536832594078,2.056279055785,2.0722830490121,2.09109201382839,
2.13125112005048,2.18749585070491,2.19857739702684,2.20505780450936,2.2114061390268,
2.22184804390554,2.23497519938454,2.26565242660347,2.33768752688447,2.35401187972869,
2.36388413422627,2.37474048669759,2.39043682060175,2.40875581975962,2.44698783953403,
2.50699268527341,2.51773193949008,2.52414078926535,2.5305531787131,2.54131076559637,
2.58832711885829,2.65531565789145,2.67222863836378,2.68330135424359,2.69323641474989,
2.70400871752801,2.71841062714054,2.73813407747398),.UNSPECIFIED.);
#73=B_SPLINE_CURVE_WITH_KNOTS('',3,(#5463,#5464,#5465,#5466,#5467),
 .UNSPECIFIED.,.F.,.F.,(4,1,4),(0.,0.98729592556514,1.11004521091133),
 .UNSPECIFIED.);
#74=B_SPLINE_CURVE_WITH_KNOTS('',3,(#5469,#5470,#5471,#5472,#5473,#5474,
#5475,#5476,#5477,#5478,#5479,#5480,#5481,#5482,#5483,#5484,#5485,#5486,
#5487,#5488,#5489,#5490,#5491,#5492,#5493,#5494,#5495,#5496,#5497,#5498,
#5499,#5500,#5501,#5502,#5503,#5504,#5505,#5506,#5507,#5508,#5509,#5510,
#5511,#5512,#5513,#5514,#5515,#5516,#5517,#5518,#5519,#5520,#5521,#5522,
#5523,#5524,#5525,#5526,#5527,#5528,#5529,#5530,#5531,#5532,#5533,#5534,
#5535,#5536,#5537,#5538,#5539,#5540,#5541,#5542,#5543,#5544,#5545,#5546,
#5547,#5548,#5549,#5550,#5551,#5552,#5553,#5554,#5555,#5556,#5557,#5558,
#5559,#5560,#5561,#5562,#5563,#5564,#5565,#5566,#5567,#5568,#5569,#5570,
#5571,#5572,#5573,#5574,#5575,#5576,#5577,#5578,#5579,#5580,#5581,#5582,
#5583,#5584,#5585,#5586,#5587,#5588,#5589,#5590,#5591,#5592,#5593,#5594,
#5595,#5596,#5597,#5598,#5599,#5600,#5601,#5602,#5603,#5604,#5605,#5606,
#5607,#5608,#5609,#5610,#5611,#5612,#5613,#5614,#5615,#5616,#5617,#5618,
#5619,#5620,#5621,#5622,#5623,#5624,#5625,#5626,#5627,#5628,#5629,#5630,
#5631,#5632,#5633,#5634,#5635,#5636,#5637,#5638,#5639,#5640,#5641,#5642,
#5643,#5644,#5645,#5646,#5647,#5648,#5649,#5650,#5651,#5652,#5653,#5654,
#5655,#5656,#5657,#5658,#5659,#5660,#5661,#5662,#5663,#5664,#5665,#5666,
#5667,#5668,#5669,#5670,#5671,#5672,#5673,#5674,#5675,#5676,#5677,#5678,
#5679,#5680,#5681,#5682,#5683,#5684,#5685),.UNSPECIFIED.,.F.,.F.,(4,3,3,
3,3,3,3,3,3,3,3,3,3,3,3,3,3,3,3,3,3,3,3,3,3,3,3,3,3,3,3,3,3,3,3,3,3,3,3,
3,3,3,3,3,3,3,3,3,3,3,3,3,3,3,3,3,3,3,3,3,3,3,3,3,3,3,3,3,3,3,3,3,4),(1.11004521091133,
1.19701335709339,1.28388235776292,1.37067611049039,1.45742933866679,1.54416470100031,
1.63090483587999,1.71772660085398,1.80458826523957,1.89159097544962,1.97459185113028,
2.06327101673013,2.15183613894509,2.24031086414059,2.33050797820994,2.41888072738085,
2.50723956600992,2.59560572419145,2.68717623731744,2.77566875995805,2.86877826832673,
2.96188777669542,3.05070298067973,3.13940823562147,3.22802697630534,3.31817156704974,
3.40669695771299,3.49521138256791,3.58373589624672,3.67509784775018,3.763754169158,
3.85646893570928,3.94918370226056,4.03781192249501,4.12632726936861,4.21475343818185,
4.30496921188733,4.39329671388509,4.48161161804857,4.56993520231051,4.66157130868931,
4.75002503908855,4.83853951085294,4.92717738846736,4.9364796278257,5.02517599892575,
5.11376021655063,5.20225588477605,5.2924458433529,5.38084394577703,5.46922973586957,
5.55762441245108,5.64916219768602,5.73768688045483,5.83073121692283,5.92377555339084,
6.0124783260962,6.10106922151394,6.18957183388173,6.27975928951601,6.36816495208386,
6.45655851974142,6.54496118346079,6.63648875733459,6.72502188060573,6.81804667978086,
6.91107147895598,7.00469257042698,7.10182705728842,7.19504650274243,7.28812775330745,
7.38103834802377,7.39323051787274),.UNSPECIFIED.);
#75=B_SPLINE_CURVE_WITH_KNOTS('',3,(#5687,#5688,#5689,#5690,#5691,#5692,
#5693,#5694,#5695,#5696,#5697,#5698,#5699,#5700,#5701,#5702,#5703,#5704,
#5705,#5706,#5707,#5708,#5709,#5710,#5711,#5712,#5713,#5714,#5715,#5716,
#5717,#5718,#5719,#5720,#5721,#5722,#5723,#5724,#5725,#5726,#5727,#5728,
#5729,#5730,#5731,#5732,#5733,#5734,#5735,#5736,#5737,#5738,#5739,#5740,
#5741,#5742,#5743,#5744,#5745,#5746,#5747,#5748,#5749,#5750,#5751,#5752,
#5753,#5754,#5755,#5756,#5757,#5758,#5759,#5760,#5761,#5762,#5763,#5764,
#5765,#5766,#5767,#5768,#5769,#5770,#5771,#5772,#5773,#5774,#5775,#5776,
#5777,#5778,#5779,#5780,#5781,#5782,#5783,#5784,#5785,#5786,#5787,#5788,
#5789,#5790,#5791,#5792,#5793,#5794,#5795,#5796,#5797,#5798,#5799,#5800,
#5801,#5802,#5803,#5804,#5805,#5806,#5807,#5808,#5809,#5810,#5811,#5812,
#5813,#5814,#5815,#5816,#5817,#5818,#5819,#5820,#5821,#5822,#5823,#5824,
#5825,#5826,#5827,#5828,#5829,#5830,#5831,#5832,#5833,#5834,#5835,#5836,
#5837,#5838,#5839,#5840,#5841,#5842,#5843,#5844,#5845,#5846,#5847,#5848,
#5849,#5850,#5851,#5852,#5853,#5854,#5855,#5856,#5857,#5858,#5859,#5860,
#5861,#5862,#5863,#5864,#5865,#5866,#5867,#5868,#5869,#5870,#5871,#5872,
#5873,#5874,#5875,#5876,#5877,#5878,#5879,#5880,#5881,#5882,#5883,#5884,
#5885,#5886,#5887,#5888,#5889,#5890,#5891,#5892,#5893,#5894,#5895,#5896,
#5897,#5898,#5899,#5900),.UNSPECIFIED.,.F.,.F.,(4,3,3,3,3,3,3,3,3,3,3,3,
3,3,3,3,3,3,3,3,3,3,3,3,3,3,3,3,3,3,3,3,3,3,3,3,3,3,3,3,3,3,3,3,3,3,3,3,
3,3,3,3,3,3,3,3,3,3,3,3,3,3,3,3,3,3,3,3,3,3,3,4),(7.39323051809092,7.48529307319253,
7.57746426680113,7.66983555106452,7.76231599136604,7.85499249188307,7.89836740452112,
7.9870599121303,8.07564033387518,8.1641322784918,8.25432365994111,8.34271824396276,
8.43110059916474,8.51949192877706,8.61103477910436,8.699556367841,8.79260984896363,
8.88566333008626,8.97435570299709,9.06293600738605,9.15142785206477,9.2416192775131,
9.33001380561846,9.41839612152961,9.50678742860532,9.59833038536684,9.68685199398323,
9.77990562481732,9.8729592556514,9.96164991525048,10.0502284761189,10.1387185494565,
10.2289106284265,10.3173033279091,10.405683797039,10.4940732412073,10.5856187262096,
10.6741384486948,10.7671968149556,10.8602551812165,10.9489467575841,11.0375262470332,
11.1260172595102,11.2162089904191,11.304602648982,11.3929840829243,11.4813744965563,
11.5729186491126,11.6614393437252,11.7544952252534,11.8475511067817,11.9362425867459,
12.0248219803444,12.1133128976455,12.2035046644832,12.2918982301909,12.3802795723187,
12.4686698952878,12.5602141795525,12.6487347872506,12.7417909097987,12.8348470323468,
12.9222626009469,13.0095667024862,13.0967750381868,13.1839306454997,13.2710559453825,
13.3581733274571,13.4453456514344,13.5325468425587,13.6198538539382,13.6764158250785),
 .UNSPECIFIED.);
#76=B_SPLINE_CURVE_WITH_KNOTS('',3,(#5902,#5903,#5904,#5905,#5906,#5907,
#5908,#5909,#5910,#5911,#5912,#5913,#5914,#5915,#5916,#5917,#5918,#5919,
#5920,#5921,#5922,#5923,#5924,#5925,#5926,#5927,#5928,#5929,#5930,#5931,
#5932,#5933,#5934,#5935,#5936,#5937,#5938,#5939,#5940,#5941,#5942,#5943,
#5944,#5945,#5946,#5947,#5948,#5949,#5950,#5951,#5952,#5953,#5954,#5955,
#5956,#5957,#5958,#5959,#5960,#5961,#5962,#5963,#5964,#5965,#5966,#5967,
#5968,#5969,#5970,#5971,#5972,#5973,#5974,#5975,#5976,#5977,#5978,#5979,
#5980,#5981,#5982,#5983,#5984,#5985,#5986,#5987,#5988,#5989,#5990,#5991,
#5992,#5993,#5994,#5995,#5996,#5997,#5998,#5999,#6000,#6001,#6002,#6003,
#6004,#6005,#6006,#6007,#6008,#6009,#6010,#6011,#6012,#6013,#6014,#6015,
#6016,#6017,#6018,#6019,#6020,#6021,#6022,#6023,#6024,#6025,#6026,#6027,
#6028,#6029,#6030,#6031,#6032,#6033,#6034,#6035,#6036,#6037,#6038,#6039,
#6040,#6041,#6042,#6043,#6044,#6045,#6046,#6047,#6048,#6049,#6050,#6051,
#6052,#6053,#6054,#6055,#6056,#6057,#6058,#6059,#6060,#6061,#6062,#6063,
#6064,#6065,#6066,#6067,#6068,#6069,#6070,#6071,#6072,#6073,#6074,#6075,
#6076,#6077,#6078,#6079,#6080,#6081,#6082,#6083,#6084,#6085,#6086,#6087,
#6088,#6089,#6090,#6091,#6092,#6093,#6094,#6095,#6096,#6097,#6098,#6099,
#6100,#6101,#6102,#6103,#6104,#6105,#6106,#6107,#6108,#6109),
 .UNSPECIFIED.,.F.,.F.,(4,3,3,3,3,3,3,3,3,3,3,3,3,3,3,3,3,3,3,3,3,3,3,3,
3,3,3,3,3,3,3,3,3,3,3,3,3,3,3,3,3,3,3,3,3,3,3,3,3,3,3,3,3,3,3,3,3,3,3,3,
3,3,3,3,3,3,3,3,3,4),(13.6764158252705,13.822142957912,13.910834385622,
13.9994137254484,14.087904587536,14.1780963745286,14.2664898818076,14.3548711644067,
14.4432614268103,14.534805790977,14.6233263360623,14.7163826097697,14.8094388834771,
14.8981302929591,14.9867096144838,15.0752004582202,15.1653922520729,15.2537857410009,
15.3421670052827,15.4305572494239,15.5221016393285,15.6106221664602,15.7036784877512,
15.7967348090422,15.8854262058353,15.9740055144055,16.0624963449394,16.1526881436479,
16.2410816188459,16.3294628692249,16.4178530993054,16.5093975081309,16.5979180209356,
16.6909743777715,16.7840307346074,16.872722141994,16.9613014613115,17.049792302732,
17.139984097412,17.2283775837697,17.3167588453903,17.4051490867822,17.4966934801298,
17.5852140043155,17.678270332244,17.7713266601725,17.8600180648758,17.948597381489,
18.0370882201877,18.1272800158815,18.2156734994925,18.3040547583622,18.3924449970019,
18.4839893941859,18.5725099156422,18.6655662506899,18.7586225857377,18.8473139894916,
18.9358933051323,19.0243841428369,19.1145759388951,19.2029694214646,19.2913506792768,
19.3797409168442,19.4712853154589,19.5598058358158,19.6528621735593,19.7459185113028,
19.8669494233805,19.9596011324501),.UNSPECIFIED.);
#77=B_SPLINE_CURVE_WITH_KNOTS('',3,(#6111,#6112,#6113,#6114,#6115,#6116,
#6117,#6118,#6119,#6120,#6121,#6122,#6123,#6124,#6125,#6126,#6127,#6128,
#6129,#6130,#6131,#6132,#6133,#6134,#6135,#6136,#6137,#6138,#6139,#6140,
#6141,#6142,#6143,#6144,#6145,#6146,#6147,#6148,#6149,#6150,#6151,#6152,
#6153,#6154,#6155,#6156,#6157,#6158,#6159,#6160,#6161,#6162,#6163,#6164,
#6165,#6166,#6167,#6168,#6169,#6170,#6171,#6172,#6173,#6174,#6175,#6176,
#6177,#6178,#6179,#6180,#6181,#6182,#6183,#6184,#6185,#6186,#6187,#6188,
#6189,#6190,#6191,#6192,#6193,#6194,#6195,#6196,#6197,#6198,#6199,#6200,
#6201,#6202,#6203,#6204,#6205,#6206,#6207,#6208,#6209,#6210,#6211,#6212,
#6213,#6214,#6215,#6216,#6217,#6218,#6219,#6220,#6221,#6222,#6223,#6224,
#6225,#6226,#6227,#6228,#6229,#6230,#6231,#6232,#6233,#6234,#6235,#6236,
#6237,#6238,#6239,#6240,#6241,#6242,#6243,#6244,#6245,#6246,#6247,#6248,
#6249,#6250,#6251,#6252,#6253,#6254,#6255,#6256,#6257,#6258,#6259,#6260,
#6261,#6262,#6263,#6264,#6265,#6266,#6267,#6268,#6269,#6270,#6271,#6272,
#6273,#6274,#6275,#6276,#6277,#6278,#6279,#6280,#6281,#6282,#6283,#6284,
#6285,#6286,#6287,#6288,#6289,#6290,#6291,#6292,#6293,#6294,#6295,#6296,
#6297,#6298,#6299,#6300,#6301,#6302,#6303,#6304,#6305,#6306,#6307,#6308,
#6309,#6310,#6311,#6312,#6313,#6314,#6315,#6316,#6317,#6318,#6319,#6320,
#6321,#6322,#6323,#6324),.UNSPECIFIED.,.F.,.F.,(4,3,3,3,3,3,3,3,3,3,3,3,
3,3,3,3,3,3,3,3,3,3,3,3,3,3,3,3,3,3,3,3,3,3,3,3,3,3,3,3,3,3,3,3,3,3,3,3,
3,3,3,3,3,3,3,3,3,3,3,3,3,3,3,3,3,3,3,3,3,3,3,4),(19.9596011326718,20.0469237800727,
20.1341771968951,20.2213938721846,20.3085961433456,20.3958063314767,20.4830999449737,
20.570435755381,20.6579098238915,20.7332144368679,20.8219058413541,20.9104851577402,
20.9989759962022,21.0891677919811,21.1775612753329,21.2659425339355,21.3543327723005,
21.4458771698336,21.5343976909983,21.6274540267157,21.7205103624331,21.809201766862,
21.8977810831887,21.9862719215897,22.0764637173908,22.1648572006777,22.253238459214,
22.3416286975111,22.4331730951328,22.5216936162272,22.6147499521127,22.7078062879982,
22.7964976925349,22.8850770089713,22.9735678474835,23.0637596432435,23.1521531266447,
23.2405343852962,23.3289246237095,23.4204690211729,23.5089895423846,23.602045877974,
23.6951022135634,23.7837936180562,23.8723729344482,23.9608637729156,24.0510555686922,
24.1394490520478,24.2278303106535,24.316220549021,24.4077649465478,24.4962854677135,
24.589341803421,24.6823981391285,24.7710895436196,24.8596688600099,24.9481596984755,
25.0383514942527,25.126744977606,25.2151262362092,25.3035164745745,25.3950608721043,
25.4835813932671,25.5766377289804,25.6696940646936,25.7601596923641,25.8504978540204,
25.9407269674771,26.0308459404358,26.1209002292553,26.2109023846584,26.2427864396297),
 .UNSPECIFIED.);
#78=B_SPLINE_CURVE_WITH_KNOTS('',3,(#6326,#6327,#6328,#6329,#6330,#6331,
#6332,#6333,#6334,#6335,#6336,#6337,#6338,#6339,#6340,#6341,#6342,#6343,
#6344,#6345,#6346,#6347,#6348,#6349,#6350,#6351,#6352,#6353,#6354,#6355,
#6356,#6357,#6358,#6359,#6360,#6361,#6362,#6363,#6364,#6365,#6366,#6367,
#6368,#6369,#6370,#6371,#6372,#6373,#6374,#6375,#6376,#6377,#6378,#6379,
#6380,#6381,#6382,#6383,#6384,#6385,#6386,#6387,#6388,#6389,#6390,#6391,
#6392,#6393,#6394,#6395,#6396,#6397,#6398,#6399,#6400,#6401,#6402,#6403,
#6404,#6405,#6406,#6407,#6408,#6409,#6410,#6411,#6412,#6413,#6414,#6415,
#6416,#6417,#6418,#6419,#6420,#6421,#6422,#6423,#6424,#6425,#6426,#6427,
#6428,#6429,#6430,#6431,#6432,#6433,#6434,#6435,#6436,#6437,#6438,#6439,
#6440,#6441,#6442,#6443,#6444,#6445,#6446,#6447,#6448,#6449,#6450,#6451,
#6452,#6453,#6454,#6455,#6456,#6457,#6458,#6459,#6460,#6461,#6462,#6463,
#6464,#6465,#6466,#6467,#6468,#6469,#6470,#6471,#6472,#6473,#6474,#6475,
#6476,#6477,#6478,#6479,#6480,#6481,#6482,#6483,#6484,#6485,#6486,#6487,
#6488,#6489,#6490,#6491,#6492,#6493,#6494,#6495,#6496,#6497,#6498,#6499,
#6500,#6501,#6502,#6503,#6504,#6505,#6506,#6507,#6508,#6509,#6510,#6511,
#6512,#6513,#6514,#6515,#6516,#6517,#6518,#6519,#6520,#6521,#6522,#6523,
#6524,#6525,#6526,#6527,#6528,#6529,#6530,#6531,#6532,#6533,#6534,#6535,
#6536,#6537,#6538,#6539),.UNSPECIFIED.,.F.,.F.,(4,3,3,3,3,3,3,3,3,3,3,3,
3,3,3,3,3,3,3,3,3,3,3,3,3,3,3,3,3,3,3,3,3,3,3,3,3,3,3,3,3,3,3,3,3,3,3,3,
3,3,3,3,3,3,3,3,3,3,3,3,3,3,3,3,3,3,3,3,3,3,3,4),(26.242786439791,26.3389678131502,
26.4355814021047,26.5324211410047,26.6295674855356,26.6569899902588,26.7456813947491,
26.8342607111387,26.9227515496036,27.0129433453811,27.1013368287343,27.1897180873376,
27.2781083257026,27.3696527232329,27.4581732443964,27.5512295801101,27.6442859158239,
27.7329773203172,27.8215566367098,27.9100474751774,28.0002392709539,28.0886327543096,
28.1770140129154,28.2654042512827,28.3569486488093,28.4454691699747,28.5385255056819,
28.6315818413891,28.7202732459279,28.808852562366,28.8973434008794,28.9875351966388,
29.0759286800403,29.1643099386917,29.2527001771046,29.344244574567,29.4327650957773,
29.5258214313657,29.6188777669542,29.7075691713759,29.7961484876969,29.8846393260935,
29.9748311218968,30.0632246051826,30.1516058637191,30.2399961020178,30.3315404996432,
30.4200610207422,30.5131173566308,30.6061736925193,30.6948650970128,30.7834444134047,
30.8719352518711,30.9621270476478,31.0505205310006,31.1389017896029,31.2272920279661,
31.3188364254957,31.4073569466556,31.5004132823701,31.5934696180845,31.6814401592432,
31.7692990613542,31.857070757937,31.9447815725409,32.0324610760959,32.1201312161915,
32.2078139283142,32.29558092047,32.3833936954151,32.4713359381952,32.5259717466392),
 .UNSPECIFIED.);
#79=B_SPLINE_CURVE_WITH_KNOTS('',3,(#6541,#6542,#6543,#6544,#6545,#6546,
#6547,#6548,#6549,#6550,#6551,#6552,#6553,#6554,#6555,#6556,#6557,#6558,
#6559,#6560,#6561,#6562,#6563,#6564,#6565,#6566,#6567,#6568,#6569,#6570,
#6571,#6572,#6573,#6574,#6575,#6576,#6577,#6578,#6579,#6580,#6581,#6582,
#6583,#6584,#6585,#6586,#6587,#6588,#6589,#6590,#6591,#6592,#6593,#6594,
#6595,#6596,#6597,#6598,#6599,#6600,#6601,#6602,#6603,#6604,#6605,#6606,
#6607,#6608,#6609,#6610,#6611,#6612,#6613,#6614,#6615,#6616,#6617,#6618,
#6619,#6620,#6621,#6622,#6623,#6624,#6625,#6626,#6627,#6628,#6629,#6630,
#6631,#6632,#6633,#6634,#6635,#6636,#6637,#6638,#6639,#6640,#6641,#6642,
#6643,#6644,#6645,#6646,#6647,#6648,#6649,#6650,#6651,#6652,#6653,#6654,
#6655,#6656,#6657,#6658,#6659,#6660,#6661,#6662,#6663,#6664,#6665,#6666,
#6667,#6668,#6669,#6670,#6671,#6672,#6673,#6674,#6675,#6676,#6677,#6678,
#6679,#6680,#6681,#6682,#6683,#6684,#6685,#6686,#6687,#6688,#6689,#6690,
#6691,#6692,#6693,#6694,#6695,#6696,#6697,#6698,#6699,#6700,#6701,#6702,
#6703,#6704,#6705,#6706,#6707,#6708,#6709,#6710,#6711,#6712,#6713,#6714,
#6715,#6716,#6717,#6718,#6719,#6720,#6721,#6722,#6723,#6724,#6725,#6726,
#6727,#6728,#6729,#6730,#6731,#6732,#6733,#6734,#6735,#6736,#6737,#6738,
#6739,#6740,#6741,#6742,#6743,#6744,#6745,#6746,#6747,#6748,#6749,#6750,
#6751),.UNSPECIFIED.,.F.,.F.,(4,3,3,3,3,3,3,3,3,3,3,3,3,3,3,3,3,3,3,3,3,
3,3,3,3,3,3,3,3,3,3,3,3,3,3,3,3,3,3,3,3,3,3,3,3,3,3,3,3,3,3,3,3,3,3,3,3,
3,3,3,3,3,3,3,3,3,3,3,3,3,4),(32.5259717468093,32.5807655436496,32.6694569473346,
32.7580362629197,32.8465271005819,32.936718896661,33.0251123792211,33.1134936370362,
33.2018838746188,33.2934282732678,33.3819487936705,33.4750051314427,33.5680614692148,
33.6567528740102,33.7453321906977,33.833823029453,33.9240148251188,34.0124083087424,
34.1007895676081,34.1891798062273,34.2807242033654,34.3692447247604,34.4623010597702,
34.5553573947799,34.6440488022623,34.7326281216572,34.8211189631364,34.9113107577875,
34.9997042441582,35.0880855057747,35.1764757471452,35.2680201404452,35.3565406645672,
35.4495969924561,35.542653320345,35.6313447164961,35.7199240245483,35.8084148546879,
35.8986066535907,35.9870001287016,36.0753813791082,36.163771609331,36.2553160184758,
36.3438365317079,36.436892888809,36.5299492459102,36.618640656464,36.7072199788533,
36.7957108232477,36.8859026167761,36.9742961058495,37.0626773700851,37.1510676139887,
37.2426120033603,37.3311325297788,37.424188850627,37.5172451714753,37.6059365995803,
37.6945159397253,37.7830068020554,37.8731985889285,37.9615920962611,38.0499733788434,
38.1383636411596,38.2299080051299,38.3184285499525,38.4114848234965,38.5045410970405,
38.6109616044168,38.7162352571934,38.8091570538353),.UNSPECIFIED.);
#80=B_SPLINE_CURVE_WITH_KNOTS('',3,(#6753,#6754,#6755,#6756,#6757,#6758,
#6759,#6760,#6761,#6762,#6763,#6764,#6765,#6766,#6767,#6768,#6769,#6770,
#6771,#6772,#6773,#6774,#6775,#6776,#6777,#6778,#6779,#6780,#6781,#6782,
#6783,#6784,#6785,#6786,#6787,#6788,#6789,#6790,#6791,#6792,#6793,#6794,
#6795,#6796,#6797,#6798,#6799,#6800,#6801,#6802,#6803,#6804,#6805,#6806,
#6807,#6808,#6809,#6810,#6811,#6812,#6813,#6814,#6815,#6816,#6817,#6818,
#6819,#6820,#6821,#6822,#6823,#6824,#6825,#6826,#6827,#6828,#6829,#6830,
#6831,#6832,#6833,#6834,#6835,#6836,#6837,#6838,#6839,#6840,#6841,#6842,
#6843,#6844,#6845,#6846,#6847,#6848,#6849,#6850,#6851,#6852,#6853,#6854,
#6855,#6856,#6857,#6858,#6859,#6860,#6861,#6862,#6863,#6864,#6865,#6866,
#6867,#6868,#6869,#6870,#6871,#6872,#6873,#6874,#6875,#6876,#6877,#6878,
#6879,#6880,#6881,#6882,#6883,#6884,#6885,#6886,#6887,#6888,#6889,#6890,
#6891,#6892,#6893,#6894,#6895,#6896,#6897,#6898,#6899,#6900,#6901,#6902,
#6903,#6904,#6905,#6906,#6907,#6908,#6909,#6910,#6911,#6912,#6913,#6914,
#6915,#6916,#6917,#6918,#6919,#6920,#6921,#6922,#6923,#6924,#6925,#6926,
#6927,#6928,#6929,#6930,#6931,#6932,#6933,#6934,#6935,#6936,#6937,#6938,
#6939,#6940,#6941,#6942,#6943,#6944,#6945,#6946,#6947,#6948,#6949,#6950,
#6951,#6952,#6953,#6954,#6955,#6956,#6957,#6958,#6959,#6960,#6961,#6962,
#6963,#6964,#6965,#6966),.UNSPECIFIED.,.F.,.F.,(4,3,3,3,3,3,3,3,3,3,3,3,
3,3,3,3,3,3,3,3,3,3,3,3,3,3,3,3,3,3,3,3,3,3,3,3,3,3,3,3,3,3,3,3,3,3,3,3,
3,3,3,3,3,3,3,3,3,3,3,3,3,3,3,3,3,3,3,3,3,3,3,4),(38.8091570539888,38.8971609962568,
38.9851394954773,39.0731141630393,39.1611066024483,39.2491930905398,39.3373291738814,
39.4256069554307,39.4918370226056,39.580528514339,39.6691079174307,39.7575988419588,
39.8477906052353,39.9361841725392,40.0245655141604,40.1129558345204,40.2045001129329,
40.2930207127995,40.3860768304851,40.4791329481707,40.5678245231247,40.6564040114336,
40.7448950230426,40.8350867543793,40.9234804127504,41.0118618467536,41.1002522606992,
41.1917964139584,41.2803171095116,41.3733729916237,41.4664288737359,41.5551194833438,
41.6436980038881,41.7321880465287,41.8223801406253,41.9107728333273,41.9991533046095,
42.0875427598615,42.1790882697214,42.2676080254717,42.3606664123863,42.453724799301,
42.5424172958676,42.6309977000003,42.7194896206085,42.8096810086407,42.8980755535172,
42.9864578641023,43.074849143759,43.1663920390358,43.2549135653677,43.347967145117,
43.4410207248662,43.529713168881,43.6182935393289,43.7067854448956,43.7969768455876,
43.8853714209839,43.973753778925,44.062145122639,44.1536880045871,44.2422096356415,
44.3352631430364,44.4283166504313,44.5168547259066,44.6052841782716,44.6936265092543,
44.7819031478381,44.870142582569,44.9583597887507,45.0465968796254,45.0923423611684),
 .UNSPECIFIED.);
#81=B_SPLINE_CURVE_WITH_KNOTS('',3,(#6968,#6969,#6970,#6971,#6972,#6973,
#6974,#6975,#6976,#6977,#6978,#6979,#6980,#6981,#6982,#6983,#6984,#6985,
#6986,#6987,#6988,#6989,#6990,#6991,#6992,#6993,#6994,#6995,#6996,#6997,
#6998,#6999,#7000,#7001,#7002,#7003,#7004,#7005,#7006,#7007,#7008,#7009,
#7010,#7011,#7012,#7013,#7014,#7015,#7016,#7017,#7018,#7019,#7020,#7021,
#7022,#7023,#7024,#7025,#7026,#7027,#7028,#7029,#7030,#7031,#7032,#7033,
#7034,#7035,#7036,#7037,#7038,#7039,#7040,#7041,#7042,#7043,#7044,#7045,
#7046,#7047,#7048,#7049,#7050,#7051,#7052,#7053,#7054,#7055,#7056,#7057,
#7058,#7059,#7060,#7061,#7062,#7063,#7064,#7065,#7066,#7067,#7068,#7069,
#7070,#7071,#7072,#7073,#7074,#7075,#7076,#7077,#7078,#7079,#7080,#7081,
#7082,#7083,#7084,#7085,#7086,#7087,#7088,#7089,#7090,#7091,#7092,#7093,
#7094,#7095,#7096,#7097,#7098,#7099,#7100,#7101,#7102,#7103,#7104,#7105,
#7106,#7107,#7108,#7109,#7110,#7111,#7112,#7113,#7114,#7115,#7116,#7117,
#7118,#7119,#7120,#7121,#7122,#7123,#7124,#7125,#7126,#7127,#7128,#7129,
#7130,#7131,#7132,#7133,#7134,#7135,#7136,#7137,#7138,#7139,#7140,#7141,
#7142,#7143,#7144,#7145,#7146,#7147,#7148),.UNSPECIFIED.,.F.,.F.,(4,3,3,
3,3,3,3,3,3,3,3,3,3,3,3,3,3,3,3,3,3,3,3,3,3,3,3,3,3,3,3,3,3,3,3,3,3,3,3,
3,3,3,3,3,3,3,3,3,3,3,3,3,3,3,3,3,3,3,3,3,4),(45.0923423613472,45.1954635567779,
45.2992248310576,45.4036717304518,45.4156125759964,45.5043166047354,45.5929085132717,
45.6814118968335,45.7715989724245,45.8600048052718,45.9483983187276,46.0368007038082,
46.1283276532466,46.216859940611,46.3098842210863,46.4029085015616,46.4916038154234,
46.5801871802618,46.6686821993189,46.7588724777948,46.8472704368479,46.9356562725042,
47.0240511835473,47.1155894944421,47.2041148807565,47.2971596539416,47.3902044271267,
47.4788295400663,47.5673423800983,47.6557666400549,47.7459833541346,47.8343104336168,
47.9226254701026,48.0109497414159,48.1025873942349,48.1910431907813,48.2795602065755,
48.3682012831507,48.3775003526918,48.4663274941079,48.5550423748666,48.6436684390571,
48.7338094189571,48.8223364205068,48.910850319811,48.9993721719169,49.0907281985019,
49.1793765648354,49.2720864215462,49.364796278257,49.4524061344098,49.5399061070432,
49.6305462355617,49.7179014996095,49.8052286593192,49.8925499496824,49.9798875964482,
50.0673084984293,50.154779220223,50.2423674345182,50.2650271351914),
 .UNSPECIFIED.);
#82=B_SPLINE_CURVE_WITH_KNOTS('',3,(#7152,#7153,#7154,#7155,#7156,#7157,
#7158,#7159),.UNSPECIFIED.,.F.,.F.,(4,1,1,1,1,4),(-52.3266840549524,-51.3393881293873,
-50.3520922038222,-49.3647962782571,-48.3775003526919,-48.075051328453),
 .UNSPECIFIED.);
#83=B_SPLINE_CURVE_WITH_KNOTS('',3,(#7161,#7162,#7163,#7164,#7165,#7166,
#7167,#7168,#7169,#7170,#7171,#7172,#7173,#7174,#7175,#7176,#7177,#7178,
#7179,#7180,#7181,#7182,#7183,#7184,#7185,#7186,#7187,#7188,#7189,#7190,
#7191,#7192,#7193,#7194,#7195,#7196,#7197,#7198,#7199,#7200,#7201,#7202,
#7203,#7204,#7205,#7206,#7207,#7208,#7209,#7210,#7211,#7212,#7213,#7214,
#7215,#7216,#7217,#7218,#7219,#7220,#7221,#7222,#7223,#7224,#7225,#7226,
#7227,#7228,#7229,#7230,#7231,#7232,#7233,#7234,#7235,#7236,#7237,#7238,
#7239,#7240,#7241,#7242,#7243,#7244,#7245,#7246,#7247,#7248,#7249,#7250,
#7251,#7252,#7253,#7254,#7255,#7256,#7257,#7258,#7259,#7260,#7261,#7262,
#7263,#7264,#7265,#7266,#7267,#7268,#7269,#7270,#7271,#7272,#7273,#7274,
#7275,#7276,#7277,#7278,#7279,#7280,#7281,#7282,#7283,#7284,#7285,#7286,
#7287,#7288,#7289,#7290,#7291,#7292,#7293,#7294,#7295,#7296,#7297,#7298,
#7299,#7300,#7301,#7302,#7303,#7304,#7305,#7306,#7307,#7308,#7309,#7310,
#7311,#7312,#7313,#7314,#7315,#7316,#7317,#7318,#7319,#7320,#7321,#7322,
#7323,#7324,#7325,#7326,#7327,#7328,#7329,#7330,#7331,#7332,#7333,#7334,
#7335,#7336,#7337,#7338,#7339,#7340,#7341,#7342,#7343,#7344,#7345,#7346,
#7347,#7348,#7349,#7350,#7351,#7352,#7353,#7354,#7355,#7356,#7357,#7358,
#7359,#7360,#7361,#7362,#7363,#7364,#7365,#7366,#7367,#7368,#7369,#7370,
#7371,#7372,#7373,#7374),.UNSPECIFIED.,.F.,.F.,(4,3,3,3,3,3,3,3,3,3,3,3,
3,3,3,3,3,3,3,3,3,3,3,3,3,3,3,3,3,3,3,3,3,3,3,3,3,3,3,3,3,3,3,3,3,3,3,3,
3,3,3,3,3,3,3,3,3,3,3,3,3,3,3,3,3,3,3,3,3,3,3,4),(-48.0750461904513,-47.9871108288014,
-47.8992019431481,-47.8112978527581,-47.7233768854568,-47.6353623691097,
-47.5472989379262,-47.4590929505688,-47.3902044271268,-47.3015080469572,
-47.2129238201834,-47.1244281427414,-47.0342381875939,-46.9458400758472,
-46.8574542764087,-46.7690595904687,-46.6775218182419,-46.5889971261679,
-46.4959528138647,-46.4029085015616,-46.3142057267072,-46.2256148290899,
-46.1371122144743,-46.0469247596645,-45.9585190947443,-45.8701255246994,
-45.78172285856,-45.6901952879191,-45.6016621621677,-45.5086373690821,-45.4156125759965,
-45.3269281466859,-45.2383558993655,-45.1498722143147,-45.0596777688293,
-44.9712916005818,-44.8829177044209,-44.7945348676157,-44.7029803133196,
-44.6144672231741,-44.5213919368027,-44.4283166504313,-44.3396241415134,
-44.2510437184474,-44.1625517724985,-44.0723603915444,-43.9839658061715,
-43.8955834496137,-43.8071921186426,-43.7156492701985,-43.6271276801083,
-43.5340742024872,-43.4410207248662,-43.3523283516816,-43.2637480470117,
-43.1752562020449,-43.0850647767019,-42.9966702482929,-42.9082879320725,
-42.819896624683,-42.7283536683375,-42.6398320593977,-42.5467784293494,
-42.4537247993011,-42.3651482619786,-42.2766806281153,-42.1883004393225,
-42.0999863100107,-42.0117102946501,-41.9234568731682,-41.8351849856978,
-41.7918608832717),.UNSPECIFIED.);
#84=B_SPLINE_CURVE_WITH_KNOTS('',3,(#7376,#7377,#7378,#7379,#7380,#7381,
#7382,#7383,#7384,#7385,#7386,#7387,#7388,#7389,#7390,#7391,#7392,#7393,
#7394,#7395,#7396,#7397,#7398,#7399,#7400,#7401,#7402,#7403,#7404,#7405,
#7406,#7407,#7408,#7409,#7410,#7411,#7412,#7413,#7414,#7415,#7416,#7417,
#7418,#7419,#7420,#7421,#7422,#7423,#7424,#7425,#7426,#7427,#7428,#7429,
#7430,#7431,#7432,#7433,#7434,#7435,#7436,#7437,#7438,#7439,#7440,#7441,
#7442,#7443,#7444,#7445,#7446,#7447,#7448,#7449,#7450,#7451,#7452,#7453,
#7454,#7455,#7456,#7457,#7458,#7459,#7460,#7461,#7462,#7463,#7464,#7465,
#7466,#7467,#7468,#7469,#7470,#7471,#7472,#7473,#7474,#7475,#7476,#7477,
#7478,#7479,#7480,#7481,#7482,#7483,#7484,#7485,#7486,#7487,#7488,#7489,
#7490,#7491,#7492,#7493,#7494,#7495,#7496,#7497,#7498,#7499,#7500,#7501,
#7502,#7503,#7504,#7505,#7506,#7507,#7508,#7509,#7510,#7511,#7512,#7513,
#7514,#7515,#7516,#7517,#7518,#7519,#7520,#7521,#7522,#7523,#7524,#7525,
#7526,#7527,#7528,#7529,#7530,#7531,#7532,#7533,#7534,#7535,#7536,#7537,
#7538,#7539,#7540,#7541,#7542,#7543,#7544,#7545,#7546,#7547,#7548,#7549,
#7550,#7551,#7552,#7553,#7554,#7555,#7556,#7557,#7558,#7559,#7560,#7561,
#7562,#7563,#7564,#7565,#7566,#7567,#7568,#7569,#7570,#7571,#7572,#7573,
#7574,#7575,#7576,#7577,#7578,#7579,#7580,#7581,#7582,#7583,#7584,#7585,
#7586,#7587,#7588,#7589),.UNSPECIFIED.,.F.,.F.,(4,3,3,3,3,3,3,3,3,3,3,3,
3,3,3,3,3,3,3,3,3,3,3,3,3,3,3,3,3,3,3,3,3,3,3,3,3,3,3,3,3,3,3,3,3,3,3,3,
3,3,3,3,3,3,3,3,3,3,3,3,3,3,3,3,3,3,3,3,3,3,3,4),(-41.7918608830911,-41.6889257523798,
-41.5853660103364,-41.4811306934174,-41.4664288737359,-41.3777372971778,
-41.2891578075365,-41.2006667948651,-41.1104750640283,-41.0220814052683,
-40.9336999711282,-40.8453095572976,-40.7537654050159,-40.6652447102054,
-40.5721888291881,-40.4791329481708,-40.3904414681829,-40.3018620745599,
-40.2133711572333,-40.1231793904049,-40.0347858246699,-39.9464044825142,
-39.8580141595162,-39.7664698752886,-39.6779492675608,-39.5848931450832,
-39.4918370226056,-39.4031456951822,-39.3145664570197,-39.2260756978358,
-39.1358838727364,-39.0474904707518,-38.959109294152,-38.8707191383343,
-38.7791746280108,-38.6906541899937,-38.5975976435171,-38.5045410970405,
-38.4158496693036,-38.32727032945,-38.2387794673349,-38.1485876803525,-38.0601941730456,
-37.9718128904184,-37.8834226279865,-37.7918782638588,-37.7033577187453,
-37.6103014451104,-37.5172451714754,-37.4285537619925,-37.3399744404667,
-37.2514835967294,-37.161291802877,-37.0728983139477,-36.9845170496646,
-36.896126805522,-36.804582415619,-36.7160618884858,-36.623005567198,-36.5299492459102,
-36.4412578491243,-36.3526785405615,-36.2641877100351,-36.1739959113238,
-36.0856024361335,-35.9972211857622,-35.9088309556895,-35.8172865468534,
-35.7287660340565,-35.6357096772008,-35.5426533203451,-35.5086755760921),
 .UNSPECIFIED.);
#85=B_SPLINE_CURVE_WITH_KNOTS('',3,(#7591,#7592,#7593,#7594,#7595,#7596,
#7597,#7598,#7599,#7600,#7601,#7602,#7603,#7604,#7605,#7606,#7607,#7608,
#7609,#7610,#7611,#7612,#7613,#7614,#7615,#7616,#7617,#7618,#7619,#7620,
#7621,#7622,#7623,#7624,#7625,#7626,#7627,#7628,#7629,#7630,#7631,#7632,
#7633,#7634,#7635,#7636,#7637,#7638,#7639,#7640,#7641,#7642,#7643,#7644,
#7645,#7646,#7647,#7648,#7649,#7650,#7651,#7652,#7653,#7654,#7655,#7656,
#7657,#7658,#7659,#7660,#7661,#7662,#7663,#7664,#7665,#7666,#7667,#7668,
#7669,#7670,#7671,#7672,#7673,#7674,#7675,#7676,#7677,#7678,#7679,#7680,
#7681,#7682,#7683,#7684,#7685,#7686,#7687,#7688,#7689,#7690,#7691,#7692,
#7693,#7694,#7695,#7696,#7697,#7698,#7699,#7700,#7701,#7702,#7703,#7704,
#7705,#7706,#7707,#7708,#7709,#7710,#7711,#7712,#7713,#7714,#7715,#7716,
#7717,#7718,#7719,#7720,#7721,#7722,#7723,#7724,#7725,#7726,#7727,#7728,
#7729,#7730,#7731,#7732,#7733,#7734,#7735,#7736,#7737,#7738,#7739,#7740,
#7741,#7742,#7743,#7744,#7745,#7746,#7747,#7748,#7749,#7750,#7751,#7752,
#7753,#7754,#7755,#7756,#7757,#7758,#7759,#7760,#7761,#7762,#7763,#7764,
#7765,#7766,#7767,#7768,#7769,#7770,#7771,#7772,#7773,#7774,#7775,#7776,
#7777,#7778,#7779,#7780,#7781,#7782,#7783,#7784,#7785,#7786,#7787,#7788,
#7789,#7790,#7791,#7792,#7793,#7794,#7795,#7796,#7797,#7798,#7799,#7800,
#7801),.UNSPECIFIED.,.F.,.F.,(4,3,3,3,3,3,3,3,3,3,3,3,3,3,3,3,3,3,3,3,3,
3,3,3,3,3,3,3,3,3,3,3,3,3,3,3,3,3,3,3,3,3,3,3,3,3,3,3,3,3,3,3,3,3,3,3,3,
3,3,3,3,3,3,3,3,3,3,3,3,3,4),(-35.5086755758622,-35.4204742205616,-35.3323832445334,
-35.2443784702568,-35.1564329342824,-35.0685181555091,-34.9806124069457,
-34.8926939733897,-34.8046873075424,-34.7166353007272,-34.6284436413324,
-34.5553573947799,-34.4666659900769,-34.378086673464,-34.2895958347657,
-34.1994040390718,-34.111010555461,-34.0226292965915,-33.934239057952,-33.8426946607677,
-33.7541741393116,-33.6611178042632,-33.5680614692148,-33.4793700654617,
-33.390790749822,-33.3022999121181,-33.2121081160596,-33.123714633491,-33.0353333756797,
-32.9469431381131,-32.8553987394972,-32.7668782191413,-32.6738218813955,
-32.5807655436497,-32.4920741388114,-32.4034948220695,-32.3150039832488,
-32.2248121876033,-32.1364187038877,-32.04803744492,-31.9596472061894,-31.8681028091632,
-31.7795822876339,-31.6865259528592,-31.5934696180845,-31.5047782135983,
-31.4161988972124,-31.3277080587505,-31.2375162629716,-31.1491227796198,
-31.0607415210174,-30.9723512826528,-30.8808068851194,-30.7922863639549,
-30.6992300282371,-30.6061736925194,-30.5174822880907,-30.4289029717636,
-30.3404121333621,-30.2502203375611,-30.1618268542744,-30.0734455957383,
-29.985055357441,-29.8935109598193,-29.8049904387251,-29.7119341028397,
-29.6188777669542,-29.5204908512767,-29.4223663703384,-29.3239283197183,
-29.2254902690982),.UNSPECIFIED.);
#86=B_SPLINE_CURVE_WITH_KNOTS('',3,(#7803,#7804,#7805,#7806,#7807,#7808,
#7809,#7810,#7811,#7812,#7813,#7814,#7815,#7816,#7817,#7818,#7819,#7820,
#7821,#7822,#7823,#7824,#7825,#7826,#7827,#7828,#7829,#7830,#7831,#7832,
#7833,#7834,#7835,#7836,#7837,#7838,#7839,#7840,#7841,#7842,#7843,#7844,
#7845,#7846,#7847,#7848,#7849,#7850,#7851,#7852,#7853,#7854,#7855,#7856,
#7857,#7858,#7859,#7860,#7861,#7862,#7863,#7864,#7865,#7866,#7867,#7868,
#7869,#7870,#7871,#7872,#7873,#7874,#7875,#7876,#7877,#7878,#7879,#7880,
#7881,#7882,#7883,#7884,#7885,#7886,#7887,#7888,#7889,#7890,#7891,#7892,
#7893,#7894,#7895,#7896,#7897,#7898,#7899,#7900,#7901,#7902,#7903,#7904,
#7905,#7906,#7907,#7908,#7909,#7910,#7911,#7912,#7913,#7914,#7915,#7916,
#7917,#7918,#7919,#7920,#7921,#7922,#7923,#7924,#7925,#7926,#7927,#7928,
#7929,#7930,#7931,#7932,#7933,#7934,#7935,#7936,#7937,#7938,#7939,#7940,
#7941,#7942,#7943,#7944,#7945,#7946,#7947,#7948,#7949,#7950,#7951,#7952,
#7953,#7954,#7955,#7956,#7957,#7958,#7959,#7960,#7961,#7962,#7963,#7964,
#7965,#7966,#7967,#7968,#7969,#7970,#7971,#7972,#7973,#7974,#7975,#7976,
#7977,#7978,#7979,#7980,#7981,#7982,#7983,#7984,#7985,#7986,#7987,#7988,
#7989,#7990,#7991,#7992,#7993,#7994,#7995,#7996,#7997,#7998,#7999,#8000,
#8001,#8002,#8003,#8004,#8005,#8006,#8007,#8008,#8009,#8010,#8011,#8012,
#8013,#8014,#8015,#8016),.UNSPECIFIED.,.F.,.F.,(4,3,3,3,3,3,3,3,3,3,3,3,
3,3,3,3,3,3,3,3,3,3,3,3,3,3,3,3,3,3,3,3,3,3,3,3,3,3,3,3,3,3,3,3,3,3,3,3,
3,3,3,3,3,3,3,3,3,3,3,3,3,3,3,3,3,3,3,3,3,3,3,4),(-29.2254902689125,-29.1359721824779,
-29.04643034499,-28.9568455388693,-28.8671374694578,-28.7773621997721,-28.6874306548523,
-28.6315818413891,-28.5428904368963,-28.4543111205044,-28.3658202820372,
-28.2756284862605,-28.1872350029049,-28.0988537442991,-28.0104635059315,
-27.9189191084046,-27.8303985872388,-27.7373422515314,-27.644285915824,
-27.555594511333,-27.4670151949429,-27.3785243564775,-27.2883325607001,
-27.1999390773468,-27.1115578187434,-27.0231675803786,-26.9316231828486,
-26.8431026616856,-26.7500463259722,-26.6569899902588,-26.5682985857523,
-26.4797192693466,-26.3912284308653,-26.3010366350939,-26.2126431517244,
-26.1242618931048,-26.0358716547238,-25.9443272572163,-25.8558067360371,
-25.7627504003654,-25.6696940646937,-25.5810026602034,-25.4924233438138,
-25.4039325053489,-25.3137407095713,-25.2253472262182,-25.1369659676149,
-25.0485757292499,-24.9570313317196,-24.8685108105561,-24.7754544748423,
-24.6823981391285,-24.5937067346351,-24.5051274182426,-24.416636579775,
-24.3264447839985,-24.2380513006428,-24.149670042037,-24.0612798036693,
-23.9697354061428,-23.8812148849775,-23.7881585492704,-23.6951022135634,
-23.607487371775,-23.5200096733413,-23.4326102403471,-23.3452667382789,
-23.2579568864533,-23.1706322164053,-23.0833009401675,-22.995900281291,
-22.9423049619356),.UNSPECIFIED.);
#87=B_SPLINE_CURVE_WITH_KNOTS('',3,(#8018,#8019,#8020,#8021,#8022,#8023,
#8024,#8025,#8026,#8027,#8028,#8029,#8030,#8031,#8032,#8033,#8034,#8035,
#8036,#8037,#8038,#8039,#8040,#8041,#8042,#8043,#8044,#8045,#8046,#8047,
#8048,#8049,#8050,#8051,#8052,#8053,#8054,#8055,#8056,#8057,#8058,#8059,
#8060,#8061,#8062,#8063,#8064,#8065,#8066,#8067,#8068,#8069,#8070,#8071,
#8072,#8073,#8074,#8075,#8076,#8077,#8078,#8079,#8080,#8081,#8082,#8083,
#8084,#8085,#8086,#8087,#8088,#8089,#8090,#8091,#8092,#8093,#8094,#8095,
#8096,#8097,#8098,#8099,#8100,#8101,#8102,#8103,#8104,#8105,#8106,#8107,
#8108,#8109,#8110,#8111,#8112,#8113,#8114,#8115,#8116,#8117,#8118,#8119,
#8120,#8121,#8122,#8123,#8124,#8125,#8126,#8127,#8128,#8129,#8130,#8131,
#8132,#8133,#8134,#8135,#8136,#8137,#8138,#8139,#8140,#8141,#8142,#8143,
#8144,#8145,#8146,#8147,#8148,#8149,#8150,#8151,#8152,#8153,#8154,#8155,
#8156,#8157,#8158,#8159,#8160,#8161,#8162,#8163,#8164,#8165,#8166,#8167,
#8168,#8169,#8170,#8171,#8172,#8173,#8174,#8175,#8176,#8177,#8178,#8179,
#8180,#8181,#8182,#8183,#8184,#8185,#8186,#8187,#8188,#8189,#8190,#8191,
#8192,#8193,#8194,#8195,#8196,#8197,#8198,#8199,#8200,#8201,#8202,#8203,
#8204,#8205,#8206,#8207,#8208,#8209,#8210,#8211,#8212,#8213,#8214,#8215,
#8216,#8217,#8218,#8219,#8220,#8221,#8222,#8223,#8224,#8225),
 .UNSPECIFIED.,.F.,.F.,(4,3,3,3,3,3,3,3,3,3,3,3,3,3,3,3,3,3,3,3,3,3,3,3,
3,3,3,3,3,3,3,3,3,3,3,3,3,3,3,3,3,3,3,3,3,3,3,3,3,3,3,3,3,3,3,3,3,3,3,3,
3,3,3,3,3,3,3,3,3,4),(-22.9423049617329,-22.8250556248655,-22.7078062879982,
-22.6191148835766,-22.5305355672557,-22.4420447288591,-22.3518529330559,
-22.2634594497701,-22.1750781912337,-22.086687952935,-21.9951435553095,
-21.9066230342105,-21.8135666983218,-21.7205103624331,-21.6318189579397,
-21.5432396415478,-21.4547488030814,-21.3645570073048,-21.276163523952,
-21.1877822653498,-21.0993920269868,-21.0078476294571,-20.9193271082973,
-20.8262707725827,-20.733214436868,-20.6445230320143,-20.5559437152602,
-20.4674528764303,-20.3772610807893,-20.2888675970716,-20.2004863381047,
-20.1120960993774,-20.0205517023588,-19.9320311808397,-19.8389748460713,
-19.7459185113028,-19.6572271076187,-19.5686477920344,-19.4801569543731,
-19.3899651582937,-19.3015716757345,-19.2131904179202,-19.1248001803384,
-19.0332557816882,-18.9447352612863,-18.851678923512,-18.7586225857377,
-18.6699311809424,-18.581351864255,-18.4928610254998,-18.4026692298339,
-18.3142757462105,-18.2258944873449,-18.1375042487258,-18.0459598515875,
-17.9574393301927,-17.8643829951826,-17.7713266601725,-17.6826352526863,
-17.5940559332877,-17.5055650918046,-17.4153732971549,-17.3269798107805,
-17.2385985491602,-17.1502083077859,-17.0586639144913,-16.9701433903655,
-16.8770870624864,-16.7840307346074,-16.6591196545534),.UNSPECIFIED.);
#88=B_SPLINE_CURVE_WITH_KNOTS('',3,(#8227,#8228,#8229,#8230,#8231,#8232,
#8233,#8234,#8235,#8236,#8237,#8238,#8239,#8240,#8241,#8242,#8243,#8244,
#8245,#8246,#8247,#8248,#8249,#8250,#8251,#8252,#8253,#8254,#8255,#8256,
#8257,#8258,#8259,#8260,#8261,#8262,#8263,#8264,#8265,#8266,#8267,#8268,
#8269,#8270,#8271,#8272,#8273,#8274,#8275,#8276,#8277,#8278,#8279,#8280,
#8281,#8282,#8283,#8284,#8285,#8286,#8287,#8288,#8289,#8290,#8291,#8292,
#8293,#8294,#8295,#8296,#8297,#8298,#8299,#8300,#8301,#8302,#8303,#8304,
#8305,#8306,#8307,#8308,#8309,#8310,#8311,#8312,#8313,#8314,#8315,#8316,
#8317,#8318,#8319,#8320,#8321,#8322,#8323,#8324,#8325,#8326,#8327,#8328,
#8329,#8330,#8331,#8332,#8333,#8334,#8335,#8336,#8337,#8338,#8339,#8340,
#8341,#8342,#8343,#8344,#8345,#8346,#8347,#8348,#8349,#8350,#8351,#8352,
#8353,#8354,#8355,#8356,#8357,#8358,#8359,#8360,#8361,#8362,#8363,#8364,
#8365,#8366,#8367,#8368,#8369,#8370,#8371,#8372,#8373,#8374,#8375,#8376,
#8377,#8378,#8379,#8380,#8381,#8382,#8383,#8384,#8385,#8386,#8387,#8388,
#8389,#8390,#8391,#8392,#8393,#8394,#8395,#8396,#8397,#8398,#8399,#8400,
#8401,#8402,#8403,#8404,#8405,#8406,#8407,#8408,#8409,#8410,#8411,#8412,
#8413,#8414,#8415,#8416,#8417,#8418,#8419,#8420,#8421,#8422,#8423,#8424,
#8425,#8426,#8427,#8428,#8429,#8430,#8431,#8432,#8433,#8434,#8435,#8436,
#8437,#8438,#8439,#8440),.UNSPECIFIED.,.F.,.F.,(4,3,3,3,3,3,3,3,3,3,3,3,
3,3,3,3,3,3,3,3,3,3,3,3,3,3,3,3,3,3,3,3,3,3,3,3,3,3,3,3,3,3,3,3,3,3,3,3,
3,3,3,3,3,3,3,3,3,3,3,3,3,3,3,3,3,3,3,3,3,3,3,4),(-16.6591196543414,-16.5717200910651,
-16.4844154992113,-16.3971811873345,-16.3099842840513,-16.2228024345668,
-16.1356133009829,-16.0483412871192,-15.9610276096757,-15.87357546279,-15.7967348090423,
-15.7080433984867,-15.6194640760958,-15.5309732317001,-15.4407814381722,
-15.3523879490976,-15.2640066848607,-15.1756164409559,-15.0840720515862,
-14.9955515251667,-14.9024952043219,-14.8094388834771,-14.7207474553443,
-14.6321681151713,-14.543677252813,-14.4534854659504,-14.3650919585897,
-14.2767106759796,-14.1883204136354,-14.0967760497045,-14.0082555048544,
-13.9151992313832,-13.822142957912,-13.7334516362746,-13.6448724027792,
-13.5563816471481,-13.4661898202979,-13.3777964190981,-13.2894152422491,
-13.2010250851483,-13.1094805719479,-13.0209601300808,-12.9279035812138,
-12.8348470323468,-12.7461555405831,-12.6575761374613,-12.5690852129039,
-12.4788934496386,-12.3904998823065,-12.302118540658,-12.2137282202711,
-12.1221839418987,-12.033663342007,-11.9406072243944,-11.8475511067817,
-11.7588595316319,-11.6702800431268,-11.5817890313202,-11.4915973000572,
-11.4032036414882,-11.3148222072874,-11.2264317931444,-11.1348876401625,
-11.0463669444147,-10.9533110628157,-10.8602551812166,-10.7667161797742,
-10.6690207217186,-10.5758796685901,-10.4828745688088,-10.3900370539,-10.3759343475515),
 .UNSPECIFIED.);
#89=B_SPLINE_CURVE_WITH_KNOTS('',3,(#8442,#8443,#8444,#8445,#8446,#8447,
#8448,#8449,#8450,#8451,#8452,#8453,#8454,#8455,#8456,#8457,#8458,#8459,
#8460,#8461,#8462,#8463,#8464,#8465,#8466,#8467,#8468,#8469,#8470,#8471,
#8472,#8473,#8474,#8475,#8476,#8477,#8478,#8479,#8480,#8481,#8482,#8483,
#8484,#8485,#8486,#8487,#8488,#8489,#8490,#8491,#8492,#8493,#8494,#8495,
#8496,#8497,#8498,#8499,#8500,#8501,#8502,#8503,#8504,#8505,#8506,#8507,
#8508,#8509,#8510,#8511,#8512,#8513,#8514,#8515,#8516,#8517,#8518,#8519,
#8520,#8521,#8522,#8523,#8524,#8525,#8526,#8527,#8528,#8529,#8530,#8531,
#8532,#8533,#8534,#8535,#8536,#8537,#8538,#8539,#8540,#8541,#8542,#8543,
#8544,#8545,#8546,#8547,#8548,#8549,#8550,#8551,#8552,#8553,#8554,#8555,
#8556,#8557,#8558,#8559,#8560,#8561,#8562,#8563,#8564,#8565,#8566,#8567,
#8568,#8569,#8570,#8571,#8572,#8573,#8574,#8575,#8576,#8577,#8578,#8579,
#8580,#8581,#8582,#8583,#8584,#8585,#8586,#8587,#8588,#8589,#8590,#8591,
#8592,#8593,#8594,#8595,#8596,#8597,#8598,#8599,#8600,#8601,#8602,#8603,
#8604,#8605,#8606,#8607,#8608,#8609,#8610,#8611,#8612,#8613,#8614,#8615,
#8616,#8617,#8618,#8619,#8620,#8621,#8622,#8623,#8624,#8625,#8626,#8627,
#8628,#8629,#8630,#8631,#8632,#8633,#8634,#8635,#8636,#8637,#8638,#8639,
#8640,#8641,#8642,#8643,#8644,#8645,#8646,#8647,#8648,#8649,#8650,#8651,
#8652,#8653,#8654,#8655),.UNSPECIFIED.,.F.,.F.,(4,3,3,3,3,3,3,3,3,3,3,3,
3,3,3,3,3,3,3,3,3,3,3,3,3,3,3,3,3,3,3,3,3,3,3,3,3,3,3,3,3,3,3,3,3,3,3,3,
3,3,3,3,3,3,3,3,3,3,3,3,3,3,3,3,3,3,3,3,3,3,3,4),(-10.3759343473738,-10.2837902926352,
-10.1915347289495,-10.0990763528878,-10.0065069835266,-9.91374116071349,
-9.87295925565141,-9.78426675875657,-9.69568635429885,-9.6071944333689,
-9.51700304545857,-9.42860850027105,-9.34022618937909,-9.25183490942041,
-9.16029201458688,-9.07177048796738,-8.97871690902682,-8.88566333008627,
-8.79697088473413,-8.70839051294174,-8.61989860602454,-8.52970720583661,
-8.44131262908495,-8.35293026978913,-8.26453892472304,-8.17299604467257,
-8.08447441228348,-7.99142090840231,-7.89836740452113,-7.8096833862846,
-7.72111147055351,-7.63262803793188,-7.54243346805989,-7.45404735558313,
-7.36567344174141,-7.2772905138185,-7.18573575510288,-7.09722239144174,
-7.00414693519887,-6.91107147895599,-6.82236744771185,-6.73377553668861,
-6.64527215066049,-6.55508507600178,-6.46667924075407,-6.37828572492622,
-6.28988333750439,-6.19835639147601,-6.10982410186788,-6.01679982762936,
-5.92377555339085,-5.83508023034925,-5.74649685627311,-5.65800182793224,
-5.56781155291893,-5.47941358452827,-5.39102773953078,-5.30263281915304,
-5.2110945213212,-5.1225691257749,-5.0295243768003,-4.93647962782571,-4.84911293708853,
-4.76185786747162,-4.67469860752171,-4.58759212279799,-4.50051596030311,
-4.41344769861368,-4.32632380717673,-4.23917101078679,-4.15191074349811,
-4.09274904038576),.UNSPECIFIED.);
#90=B_SPLINE_CURVE_WITH_KNOTS('',3,(#8657,#8658,#8659,#8660,#8661,#8662,
#8663,#8664,#8665,#8666,#8667,#8668,#8669,#8670,#8671,#8672,#8673,#8674,
#8675,#8676,#8677,#8678,#8679,#8680,#8681,#8682,#8683,#8684,#8685,#8686,
#8687,#8688,#8689,#8690,#8691,#8692,#8693,#8694,#8695,#8696,#8697,#8698,
#8699,#8700,#8701,#8702,#8703,#8704,#8705,#8706,#8707,#8708,#8709,#8710,
#8711,#8712,#8713,#8714,#8715,#8716,#8717,#8718,#8719,#8720,#8721,#8722,
#8723,#8724,#8725,#8726),.UNSPECIFIED.,.F.,.F.,(4,3,3,3,3,3,3,3,3,3,3,3,
3,3,3,3,3,3,3,3,3,3,3,4),(-4.09274904019418,-3.94918370226056,-3.86035654056811,
-3.77164163979092,-3.68301555586337,-3.59287458346738,-3.50434756300603,
-3.41583364513408,-3.32731177482659,-3.23595577529379,-3.14730739184115,
-3.05459758426828,-2.96188777669542,-2.87427787878097,-2.78677785774721,
-2.69608082521827,-2.60872550184669,-2.52139825894373,-2.43407686158953,
-2.34673908408296,-2.25931792435971,-2.17184692832522,-2.08425819340456,
-2.06120159751572),.UNSPECIFIED.);
#91=B_SPLINE_CURVE_WITH_KNOTS('',3,(#8727,#8728,#8729,#8730),
 .UNSPECIFIED.,.F.,.F.,(4,4),(-0.072372269045696,0.),.UNSPECIFIED.);
#92=B_SPLINE_CURVE_WITH_KNOTS('',3,(#8733,#8734,#8735,#8736,#8737,#8738,
#8739,#8740,#8741,#8742,#8743,#8744,#8745,#8746,#8747,#8748,#8749,#8750,
#8751,#8752,#8753,#8754,#8755,#8756,#8757,#8758,#8759,#8760,#8761,#8762,
#8763,#8764,#8765,#8766,#8767,#8768,#8769,#8770,#8771,#8772,#8773,#8774,
#8775,#8776,#8777,#8778,#8779,#8780,#8781,#8782,#8783,#8784,#8785,#8786,
#8787,#8788,#8789,#8790,#8791,#8792,#8793,#8794,#8795,#8796,#8797,#8798,
#8799,#8800,#8801,#8802,#8803,#8804,#8805,#8806,#8807,#8808,#8809,#8810,
#8811,#8812,#8813,#8814,#8815,#8816,#8817,#8818,#8819,#8820,#8821,#8822,
#8823,#8824,#8825,#8826,#8827,#8828,#8829,#8830,#8831,#8832,#8833,#8834,
#8835,#8836,#8837,#8838,#8839,#8840,#8841,#8842,#8843,#8844,#8845,#8846),
 .UNSPECIFIED.,.F.,.F.,(4,2,2,2,2,2,2,2,2,2,2,2,2,2,2,2,2,2,2,2,2,2,2,2,
2,2,2,2,2,2,2,2,2,2,2,2,2,2,2,2,2,2,2,2,2,2,2,2,2,2,2,2,2,2,2,2,4),(0.00517588011749154,
0.0875141621631935,0.1072706806158,0.123898613541391,0.134977664171004,
0.146087914916193,0.162900557465675,0.228641946111849,0.261168889263247,
0.274746197705738,0.285471908997522,0.291939864102497,0.298462335881067,
0.309614023097136,0.364820704487681,0.425322433259706,0.441105163970217,
0.452019069280532,0.46194567537565,0.478373502018443,0.549934333746339,
0.580819940517539,0.594012306981921,0.604502551232618,0.61087812943858,
0.617336449958275,0.628377441025916,0.685194213828864,0.725105755974606,
0.743833800434163,0.759770403011422,0.770632792912601,0.781704316206637,
0.798789989678684,0.864256114052101,0.914045413230296,0.924124080113808,
0.930380572452451,0.936930425784211,0.94835586165298,0.997887594077727,
1.04205592407398,1.06182765375212,1.07843147619386,1.0894570464359,1.10047842456566,
1.11706052554884,1.19615510002758,1.22179936635024,1.2385511971755,1.24609236952287,
1.2520834659821,1.26001903276934,1.27804395155722,1.33884421240203,1.36947904313667,
1.36958410658186),.UNSPECIFIED.);
#93=B_SPLINE_CURVE_WITH_KNOTS('',3,(#8850,#8851,#8852,#8853,#8854,#8855,
#8856,#8857,#8858,#8859,#8860,#8861,#8862,#8863,#8864,#8865,#8866,#8867,
#8868,#8869,#8870,#8871,#8872,#8873,#8874,#8875,#8876,#8877,#8878,#8879,
#8880),.UNSPECIFIED.,.F.,.F.,(4,3,3,3,3,3,3,3,3,3,4),(59.6902604184353,
59.7850915941644,59.8797805115036,59.974985048167,60.0694493384788,60.1638535857091,
60.2582198196451,60.3540190659364,60.4484022729338,60.5449095388721,60.6414168048105),
 .UNSPECIFIED.);
#94=B_SPLINE_CURVE_WITH_KNOTS('',3,(#8881,#8882,#8883,#8884,#8885,#8886,
#8887,#8888,#8889,#8890,#8891,#8892,#8893,#8894,#8895,#8896,#8897,#8898,
#8899,#8900,#8901,#8902,#8903,#8904,#8905,#8906,#8907,#8908,#8909,#8910,
#8911,#8912,#8913,#8914,#8915,#8916,#8917,#8918,#8919,#8920,#8921,#8922,
#8923,#8924,#8925,#8926,#8927,#8928,#8929,#8930,#8931,#8932,#8933,#8934,
#8935,#8936,#8937,#8938,#8939,#8940,#8941,#8942,#8943,#8944,#8945,#8946,
#8947,#8948,#8949,#8950,#8951,#8952,#8953),.UNSPECIFIED.,.F.,.F.,(4,3,3,
3,3,3,3,3,3,3,3,3,3,3,3,3,3,3,3,3,3,3,3,3,4),(57.6437844487799,57.679529028115,
57.7727160127017,57.8657816296418,57.9587533150178,58.0516627927366,58.1445408088069,
58.2374120244759,58.3303010886529,58.4232905025462,58.5163345053069,58.6095286199085,
58.6668249536802,58.7594480760478,58.8519476038469,58.9443517374887,59.0366938367222,
59.1290047385551,59.2213097753034,59.3136342681026,59.406065060458,59.4985528952185,
59.5912004323442,59.6541208792453,59.6902604182061),.UNSPECIFIED.);
#95=B_SPLINE_CURVE_WITH_KNOTS('',3,(#9178,#9179,#9180,#9181,#9182,#9183,
#9184,#9185,#9186,#9187,#9188,#9189,#9190,#9191,#9192,#9193,#9194,#9195,
#9196,#9197,#9198,#9199,#9200,#9201,#9202,#9203,#9204,#9205,#9206,#9207,
#9208,#9209,#9210,#9211,#9212,#9213,#9214,#9215,#9216,#9217,#9218,#9219,
#9220,#9221,#9222,#9223,#9224,#9225,#9226,#9227,#9228,#9229,#9230,#9231,
#9232,#9233,#9234,#9235,#9236,#9237,#9238,#9239,#9240,#9241,#9242,#9243,
#9244,#9245,#9246,#9247,#9248,#9249,#9250,#9251,#9252,#9253,#9254,#9255,
#9256,#9257,#9258,#9259,#9260,#9261,#9262,#9263,#9264,#9265,#9266,#9267,
#9268,#9269,#9270,#9271,#9272,#9273,#9274),.UNSPECIFIED.,.F.,.F.,(4,3,3,
3,3,3,3,3,3,3,3,3,3,3,3,3,3,3,3,3,3,3,3,3,3,3,3,3,3,3,3,3,4),(0.,0.0341321776409722,
0.0705192623706805,0.107542570976747,0.144565879582813,0.149931073663995,
0.155296491832842,0.191163208000379,0.227007229395259,0.262199303377544,
0.280217642131302,0.294754884682934,0.299547789786458,0.334097809215398,
0.367754528664766,0.40125928746162,0.405952789054922,0.427105611562154,
0.435491119142354,0.439986573782363,0.473632216631017,0.507584951788435,
0.54129439870138,0.566464885397458,0.571999583646233,0.605097850922722,
0.637624306629265,0.65106250367107,0.658566610550264,0.664632956637089,
0.696440307584404,0.727381547156091,0.744397949170633),.UNSPECIFIED.);
#96=B_SPLINE_CURVE_WITH_KNOTS('',3,(#9275,#9276,#9277,#9278,#9279,#9280,
#9281,#9282,#9283,#9284,#9285,#9286,#9287,#9288,#9289,#9290,#9291,#9292,
#9293,#9294,#9295,#9296,#9297,#9298,#9299,#9300,#9301,#9302,#9303,#9304,
#9305,#9306,#9307,#9308,#9309,#9310,#9311,#9312,#9313,#9314,#9315,#9316,
#9317,#9318,#9319,#9320,#9321,#9322,#9323,#9324,#9325,#9326,#9327,#9328,
#9329,#9330,#9331,#9332,#9333,#9334,#9335,#9336,#9337,#9338,#9339,#9340,
#9341,#9342,#9343,#9344,#9345,#9346,#9347,#9348,#9349,#9350,#9351,#9352,
#9353,#9354,#9355,#9356,#9357,#9358,#9359,#9360,#9361,#9362,#9363,#9364,
#9365,#9366,#9367,#9368,#9369,#9370,#9371),.UNSPECIFIED.,.F.,.F.,(4,3,3,
3,3,3,3,3,3,3,3,3,3,3,3,3,3,3,3,3,3,3,3,3,3,3,3,3,3,3,3,3,4),(-0.744397949170565,
-0.716065321046432,-0.684738321171649,-0.6654500864001,-0.659676869837572,
-0.653635757178455,-0.621601508366302,-0.588770968384987,-0.576827016705555,
-0.571499825003365,-0.56657139186745,-0.533059953254888,-0.499151341272541,
-0.46530750476424,-0.442807387674953,-0.437357263297704,-0.433075739176151,
-0.398167633212208,-0.37462939230316,-0.340534007097898,-0.306438621892637,
-0.298945074622502,-0.291596664676506,-0.256768715632937,-0.221366271582615,
-0.185516523185835,-0.155715905664787,-0.150803540172397,-0.145702635476358,
-0.108970996938497,-0.0721764084372337,-0.0360779656303773,0.),
 .UNSPECIFIED.);
#97=B_SPLINE_CURVE_WITH_KNOTS('',3,(#9373,#9374,#9375,#9376,#9377,#9378,
#9379,#9380,#9381,#9382,#9383,#9384,#9385,#9386,#9387,#9388,#9389,#9390,
#9391,#9392,#9393,#9394,#9395,#9396,#9397,#9398,#9399,#9400,#9401,#9402,
#9403,#9404,#9405,#9406,#9407,#9408,#9409,#9410,#9411,#9412,#9413,#9414,
#9415,#9416,#9417,#9418,#9419,#9420,#9421,#9422,#9423,#9424,#9425,#9426,
#9427,#9428,#9429,#9430,#9431,#9432,#9433,#9434,#9435,#9436,#9437,#9438,
#9439,#9440,#9441,#9442,#9443,#9444,#9445,#9446,#9447,#9448,#9449,#9450,
#9451,#9452,#9453,#9454,#9455,#9456,#9457,#9458,#9459,#9460),
 .UNSPECIFIED.,.F.,.F.,(4,3,3,3,3,3,3,3,3,3,3,3,3,3,3,3,3,3,3,3,3,3,3,3,
3,3,3,3,3,4),(-0.733997891590042,-0.707293145123096,-0.670548287271981,
-0.642147796310554,-0.636048214010822,-0.599925325890975,-0.563776896277331,
-0.543414361784613,-0.537860670969721,-0.502475354749529,-0.46734667480714,
-0.433107818857019,-0.409213763332795,-0.400709630257953,-0.394895586282691,
-0.361258743023151,-0.3374092393429,-0.303003250040855,-0.268725072296995,
-0.262744346017593,-0.256126575954077,-0.222699029434053,-0.189225882444478,
-0.156353015875858,-0.127820019143976,-0.123154998639534,-0.0909627469967315,
-0.0592242090186183,-0.0284625885623667,-1.98144071232518E-14),
 .UNSPECIFIED.);
#98=B_SPLINE_CURVE_WITH_KNOTS('',3,(#9686,#9687,#9688,#9689,#9690,#9691,
#9692,#9693,#9694,#9695,#9696,#9697,#9698,#9699,#9700,#9701,#9702,#9703,
#9704,#9705,#9706,#9707,#9708,#9709,#9710,#9711,#9712,#9713,#9714,#9715,
#9716,#9717,#9718,#9719,#9720,#9721,#9722,#9723,#9724,#9725,#9726,#9727,
#9728,#9729,#9730,#9731,#9732,#9733,#9734,#9735,#9736,#9737,#9738,#9739,
#9740,#9741,#9742,#9743,#9744,#9745,#9746,#9747,#9748,#9749,#9750,#9751,
#9752,#9753,#9754,#9755,#9756,#9757,#9758,#9759,#9760,#9761,#9762,#9763,
#9764,#9765,#9766,#9767,#9768,#9769,#9770,#9771,#9772,#9773,#9774,#9775,
#9776,#9777,#9778,#9779),.UNSPECIFIED.,.F.,.F.,(4,3,3,3,3,3,3,3,3,3,3,3,
3,3,3,3,3,3,3,3,3,3,3,3,3,3,3,3,3,3,3,4),(0.,0.0282467707211759,0.0592219961171841,
0.0911380280626913,0.123004042670125,0.127503949869102,0.132209344868245,
0.164838598782075,0.19801075530928,0.231513292775733,0.24872740517319,0.259243491625486,
0.263909575847483,0.298276876796931,0.333438871725855,0.368600866654779,
0.391892735514256,0.397647024497331,0.4032074794018,0.437128166042211,0.47167569725459,
0.506916270840531,0.535816784344498,0.541150939210018,0.546425336305492,
0.58238966892319,0.6186029543621,0.634791593471035,0.645487823943227,0.682320445220175,
0.718671345234703,0.741270768406407),.UNSPECIFIED.);
#99=B_SPLINE_CURVE_WITH_KNOTS('',3,(#9780,#9781,#9782,#9783),
 .UNSPECIFIED.,.F.,.F.,(4,4),(0.,0.0132617047994356),.UNSPECIFIED.);
#100=B_SPLINE_CURVE_WITH_KNOTS('',3,(#9842,#9843,#9844,#9845,#9846,#9847,
#9848,#9849,#9850,#9851,#9852,#9853,#9854,#9855,#9856,#9857,#9858,#9859,
#9860,#9861,#9862,#9863,#9864,#9865,#9866,#9867,#9868,#9869,#9870,#9871,
#9872,#9873,#9874,#9875,#9876,#9877,#9878,#9879,#9880,#9881,#9882,#9883,
#9884,#9885,#9886,#9887,#9888,#9889,#9890,#9891,#9892,#9893,#9894,#9895,
#9896,#9897,#9898,#9899,#9900,#9901,#9902,#9903,#9904,#9905,#9906,#9907,
#9908,#9909,#9910,#9911,#9912,#9913,#9914,#9915,#9916,#9917,#9918,#9919,
#9920,#9921,#9922,#9923),.UNSPECIFIED.,.F.,.F.,(4,3,3,3,3,3,3,3,3,3,3,3,
3,3,3,3,3,3,3,3,3,3,3,3,3,3,3,4),(-2.06741991825068,-1.98285131338516,-1.88559013949774,
-1.77615559465644,-1.68790443753717,-1.60974818243148,-1.53676333066918,
-1.46730179083953,-1.4010195987632,-1.3378649598913,-1.27712721666041,-1.21746070099515,
-1.15761317028239,-1.09756920913897,-1.03668973178852,-0.971602936806244,
-0.902947147892858,-0.830652039518071,-0.754808243576467,-0.676131879378777,
-0.596648141755566,-0.518810466257096,-0.437949267560199,-0.352276201339158,
-0.261252153029477,-0.169810646360919,-0.0802964651905899,0.),
 .UNSPECIFIED.);
#101=B_SPLINE_CURVE_WITH_KNOTS('',3,(#9927,#9928,#9929,#9930,#9931,#9932,
#9933,#9934,#9935,#9936,#9937,#9938,#9939,#9940,#9941,#9942,#9943,#9944,
#9945,#9946,#9947,#9948,#9949,#9950,#9951,#9952,#9953,#9954,#9955,#9956,
#9957,#9958,#9959,#9960,#9961,#9962,#9963,#9964,#9965,#9966,#9967,#9968,
#9969,#9970,#9971,#9972,#9973,#9974,#9975,#9976,#9977,#9978,#9979,#9980,
#9981,#9982,#9983,#9984,#9985,#9986,#9987,#9988,#9989,#9990,#9991,#9992,
#9993,#9994,#9995,#9996,#9997,#9998,#9999,#10000,#10001,#10002,#10003,#10004,
#10005,#10006,#10007,#10008,#10009,#10010,#10011,#10012,#10013,#10014,#10015,
#10016,#10017,#10018,#10019,#10020,#10021,#10022,#10023,#10024,#10025,#10026,
#10027,#10028,#10029,#10030,#10031,#10032,#10033,#10034,#10035,#10036,#10037,
#10038,#10039,#10040,#10041,#10042,#10043,#10044,#10045,#10046,#10047,#10048,
#10049,#10050,#10051,#10052,#10053,#10054,#10055,#10056,#10057,#10058,#10059,
#10060,#10061,#10062,#10063,#10064,#10065,#10066,#10067,#10068,#10069,#10070,
#10071,#10072,#10073,#10074,#10075,#10076,#10077,#10078,#10079,#10080,#10081,
#10082,#10083,#10084,#10085,#10086,#10087,#10088,#10089,#10090,#10091,#10092,
#10093,#10094,#10095,#10096,#10097,#10098,#10099,#10100,#10101,#10102,#10103,
#10104,#10105,#10106,#10107,#10108,#10109,#10110,#10111,#10112,#10113,#10114,
#10115,#10116,#10117,#10118,#10119,#10120,#10121,#10122,#10123,#10124,#10125,
#10126,#10127,#10128,#10129,#10130,#10131,#10132,#10133,#10134,#10135,#10136,
#10137,#10138,#10139,#10140,#10141,#10142,#10143,#10144,#10145,#10146,#10147,
#10148,#10149),.UNSPECIFIED.,.F.,.F.,(4,3,3,3,3,3,3,3,3,3,3,3,3,3,3,3,3,
3,3,3,3,3,3,3,3,3,3,3,3,3,3,3,3,3,3,3,3,3,3,3,3,3,3,3,3,3,3,3,3,3,3,3,3,
3,3,3,3,3,3,3,3,3,3,3,3,3,3,3,3,3,3,3,3,3,4),(-5.48556059930356,-5.3742901434944,
-5.26503542580367,-5.1577836872572,-5.04847386928929,-4.94641423339456,
-4.84632584686655,-4.74823870879311,-4.65217176427579,-4.55995510908532,
-4.49079261769247,-4.48335167319748,-4.47546446159234,-4.42482571833493,
-4.37539535138974,-4.32789456523567,-4.28330514351393,-4.22386198589148,
-4.16367959879141,-4.11102001007885,-4.0879814400171,-4.07451117436979,
-4.06881777499082,-4.06396069374141,-4.01960604117804,-3.97171900412971,
-3.91910957291902,-3.86588690476172,-3.81609285440557,-3.7976703630769,
-3.7838534945804,-3.78018597444469,-3.74240288909089,-3.68720132020267,
-3.63214582482016,-3.58397226636046,-3.54161995271181,-3.50476212826565,
-3.48863683007046,-3.48328860908609,-3.47990706616965,-3.42477351581283,
-3.36626643116087,-3.30651189415172,-3.25207197124738,-3.24675735714258,
-3.20212792397615,-3.15620343761748,-3.10888467447819,-3.06005777462237,
-3.00959125336058,-2.9774459670657,-2.96187559401661,-2.95363335797171,
-2.94977181559791,-2.80448949951976,-2.65815449920403,-2.51096234105158,
-2.36291829657365,-2.21466098559846,-2.06653880208347,-1.98094209192433,
-1.80620872497199,-1.61914703673255,-1.40683918645954,-1.18478189892939,
-1.00215186108193,-0.839832576136721,-0.690457992737357,-0.550511129775,
-0.421119097329167,-0.296518986825456,-0.178327808264077,-0.0898716726840916,
-0.0508038206324297),.UNSPECIFIED.);
#102=B_SPLINE_CURVE_WITH_KNOTS('',3,(#10159,#10160,#10161,#10162,#10163,
#10164,#10165,#10166,#10167,#10168,#10169,#10170,#10171,#10172,#10173,#10174,
#10175,#10176,#10177,#10178,#10179,#10180,#10181,#10182,#10183,#10184,#10185,
#10186,#10187,#10188,#10189,#10190,#10191,#10192,#10193,#10194,#10195,#10196,
#10197,#10198,#10199,#10200,#10201,#10202,#10203,#10204,#10205,#10206,#10207,
#10208,#10209,#10210,#10211,#10212,#10213,#10214,#10215,#10216,#10217,#10218,
#10219,#10220,#10221,#10222,#10223,#10224,#10225,#10226,#10227,#10228,#10229,
#10230,#10231,#10232,#10233,#10234,#10235,#10236,#10237,#10238,#10239,#10240,
#10241,#10242,#10243,#10244,#10245,#10246,#10247,#10248,#10249,#10250,#10251,
#10252,#10253,#10254,#10255,#10256,#10257,#10258,#10259,#10260,#10261,#10262,
#10263,#10264,#10265,#10266,#10267,#10268,#10269,#10270,#10271,#10272,#10273,
#10274,#10275,#10276,#10277,#10278,#10279,#10280,#10281,#10282,#10283,#10284,
#10285,#10286,#10287,#10288,#10289,#10290,#10291,#10292,#10293,#10294,#10295,
#10296,#10297,#10298,#10299,#10300,#10301,#10302,#10303,#10304,#10305,#10306),
 .UNSPECIFIED.,.F.,.F.,(4,3,3,3,3,3,3,3,3,3,3,3,3,3,3,3,3,3,3,3,3,3,3,3,
3,3,3,3,3,3,3,3,3,3,3,3,3,3,3,3,3,3,3,3,3,3,3,3,3,4),(-9.10855960492281,
-8.53921958763157,-8.00869400174604,-7.76001013336219,-7.63955388461377,
-7.56405433243604,-7.52369479269779,-7.50080752596703,-7.07650861767828,
-6.72947065932967,-6.625116589863,-6.56600757594707,-6.53309864263095,-6.50820482569483,
-6.14678803531956,-5.8044120104252,-5.71451198234767,-5.68978334933782,
-5.67339715853821,-5.3117835102232,-4.98297267917569,-4.82884260212217,
-4.75418584604937,-4.72996428359645,-4.70456344497697,-4.32299778199833,
-3.91934735473528,-3.47804282231225,-3.37094180328571,-3.35701328282335,
-3.17572752382557,-2.99394470365639,-2.80883622817471,-2.61893869722417,
-2.42004735513258,-2.20439292822488,-1.94398198484001,-1.70733551341788,
-1.50026985092353,-1.31908739624096,-1.16055274839372,-1.01261022609456,
-0.870637451570371,-0.733373124428186,-0.599882166408188,-0.4695171211688,
-0.342516273201481,-0.216889573446191,-0.0922346720977524,-0.0508102134630154),
 .UNSPECIFIED.);
#103=B_SPLINE_CURVE_WITH_KNOTS('',3,(#10309,#10310,#10311,#10312,#10313,
#10314,#10315,#10316,#10317,#10318,#10319,#10320,#10321,#10322,#10323,#10324,
#10325,#10326,#10327,#10328,#10329,#10330,#10331,#10332,#10333,#10334,#10335,
#10336,#10337,#10338,#10339,#10340,#10341,#10342,#10343,#10344,#10345,#10346,
#10347,#10348,#10349,#10350,#10351,#10352,#10353,#10354,#10355,#10356,#10357,
#10358,#10359,#10360,#10361,#10362,#10363,#10364,#10365,#10366,#10367,#10368,
#10369,#10370,#10371,#10372,#10373,#10374,#10375,#10376,#10377,#10378,#10379,
#10380,#10381,#10382,#10383,#10384,#10385,#10386,#10387,#10388,#10389,#10390,
#10391,#10392,#10393,#10394,#10395,#10396,#10397,#10398,#10399,#10400,#10401,
#10402,#10403,#10404,#10405,#10406,#10407,#10408,#10409,#10410,#10411,#10412,
#10413,#10414,#10415,#10416,#10417,#10418,#10419,#10420,#10421,#10422,#10423,
#10424,#10425,#10426,#10427,#10428,#10429,#10430,#10431,#10432,#10433,#10434,
#10435,#10436,#10437,#10438,#10439,#10440,#10441,#10442,#10443,#10444,#10445,
#10446,#10447,#10448,#10449,#10450,#10451,#10452,#10453,#10454,#10455,#10456,
#10457,#10458,#10459,#10460,#10461,#10462,#10463,#10464,#10465,#10466,#10467,
#10468,#10469,#10470,#10471,#10472,#10473,#10474,#10475,#10476,#10477,#10478,
#10479,#10480,#10481,#10482,#10483,#10484,#10485,#10486,#10487,#10488,#10489,
#10490,#10491,#10492,#10493,#10494,#10495,#10496,#10497,#10498,#10499,#10500,
#10501,#10502,#10503,#10504,#10505,#10506,#10507,#10508,#10509,#10510,#10511,
#10512,#10513,#10514,#10515,#10516,#10517,#10518,#10519,#10520,#10521,#10522,
#10523,#10524,#10525,#10526,#10527,#10528,#10529,#10530,#10531,#10532,#10533,
#10534,#10535,#10536,#10537,#10538,#10539,#10540,#10541,#10542,#10543),
 .UNSPECIFIED.,.F.,.F.,(4,3,3,3,3,3,3,3,3,3,3,3,3,3,3,3,3,3,3,3,3,3,3,3,
3,3,3,3,3,3,3,3,3,3,3,3,3,3,3,3,3,3,3,3,3,3,3,3,3,3,3,3,3,3,3,3,3,3,3,3,
3,3,3,3,3,3,3,3,3,3,3,3,3,3,3,3,3,3,4),(-2.02127869660357,-1.98943301980102,
-1.90463341590351,-1.81753768881889,-1.72704367650355,-1.63130693910596,
-1.51951582960439,-1.38310822332673,-1.26646899428466,-1.24459913883927,
-1.23346627262239,-1.22758843562283,-1.22207812234324,-1.15025709426344,
-1.08179540629444,-1.01496797201,-0.950320490610193,-0.916551307158433,
-0.853832223783638,-0.792204136679497,-0.731660192212863,-0.672186959028124,
-0.613766411128121,-0.590013602117237,-0.579621748174975,-0.57475056663954,
-0.571134341312111,-0.569460165760368,-0.547675695632619,-0.526546111795004,
-0.506025620571326,-0.485455200188757,-0.466281411555601,-0.447521496264729,
-0.429320222384578,-0.42374393904105,-0.399392451378572,-0.374499279646305,
-0.361614191206241,-0.358455047560918,-0.356511913591946,-0.35473329500815,
-0.344318954647855,-0.334029402325209,-0.323701337929739,-0.313256768851862,
-0.302559895706747,-0.291964358202782,-0.281691465164288,-0.279957855794893,
-0.278600543326745,-0.271418572125793,-0.262582752193856,-0.253672103340293,
-0.245540273158529,-0.238031151837375,-0.230909539922171,-0.226625838952106,
-0.216671112747294,-0.205500677732474,-0.193363451631138,-0.179480016034121,
-0.176626080324589,-0.166163697812807,-0.160971082256157,-0.159162329434394,
-0.157259342194023,-0.144809310782755,-0.13207070022678,-0.119040767714878,
-0.10571865453773,-0.091955933688298,-0.0779231319105442,-0.0636219003870916,
-0.0490527186804175,-0.034085309706883,-0.0188794529916116,-0.00332468735320998,
0.),.UNSPECIFIED.);
#104=B_SPLINE_CURVE_WITH_KNOTS('',5,(#10597,#10598,#10599,#10600,#10601,
#10602,#10603,#10604,#10605,#10606,#10607,#10608,#10609,#10610,#10611,#10612),
 .UNSPECIFIED.,.F.,.F.,(6,1,1,1,1,1,1,1,1,1,1,6),(0.481836522428161,0.5,
0.55,0.6,0.65,0.7,0.75,0.8,0.85,0.9,0.95,0.997783576468117),
 .UNSPECIFIED.);
#105=B_SPLINE_CURVE_WITH_KNOTS('',5,(#10614,#10615,#10616,#10617,#10618,
#10619,#10620,#10621,#10622,#10623,#10624,#10625,#10626,#10627,#10628),
 .UNSPECIFIED.,.F.,.F.,(6,1,1,1,1,1,1,1,1,1,6),(0.,0.05,0.1,0.15,0.2,0.25,
0.3,0.35,0.4,0.45,0.481836522428277),.UNSPECIFIED.);
#106=B_SPLINE_CURVE_WITH_KNOTS('',3,(#10632,#10633,#10634,#10635,#10636,
#10637,#10638,#10639,#10640,#10641,#10642,#10643,#10644,#10645,#10646,#10647,
#10648,#10649,#10650,#10651,#10652,#10653,#10654,#10655,#10656,#10657,#10658,
#10659,#10660,#10661,#10662,#10663,#10664,#10665,#10666,#10667,#10668,#10669,
#10670,#10671,#10672,#10673,#10674,#10675,#10676,#10677,#10678,#10679,#10680,
#10681,#10682,#10683,#10684,#10685,#10686,#10687,#10688,#10689,#10690,#10691,
#10692,#10693,#10694,#10695),.UNSPECIFIED.,.F.,.F.,(4,3,3,3,3,3,3,3,3,3,
3,3,3,3,3,3,3,3,3,3,3,4),(-0.481836522428277,-0.45532349494856,-0.432546979219204,
-0.411758376367504,-0.392204877029118,-0.373446283655192,-0.35531022111101,
-0.337405801369786,-0.319166348359288,-0.3005346337047,-0.281334526323306,
-0.261758757819788,-0.241752343726884,-0.221237113369723,-0.200124506192356,
-0.178341717407575,-0.155289187104983,-0.131213486522262,-0.105793029252951,
-0.0769868283461338,-0.0445183707397895,0.),.UNSPECIFIED.);
#107=B_SPLINE_CURVE_WITH_KNOTS('',3,(#10697,#10698,#10699,#10700,#10701,
#10702,#10703,#10704,#10705,#10706,#10707,#10708,#10709,#10710,#10711,#10712,
#10713,#10714,#10715,#10716,#10717,#10718,#10719,#10720,#10721,#10722,#10723,
#10724,#10725,#10726,#10727,#10728,#10729,#10730,#10731,#10732,#10733,#10734,
#10735,#10736,#10737,#10738,#10739,#10740,#10741,#10742,#10743,#10744,#10745,
#10746,#10747,#10748,#10749,#10750,#10751,#10752,#10753,#10754,#10755,#10756,
#10757,#10758,#10759,#10760,#10761,#10762,#10763,#10764,#10765,#10766,#10767,
#10768,#10769,#10770,#10771,#10772),.UNSPECIFIED.,.F.,.F.,(4,3,3,3,3,3,
3,3,3,3,3,3,3,3,3,3,3,3,3,3,3,3,3,3,3,4),(-1.78233413254146,-1.68011036101728,
-1.59770235095047,-1.52404961693638,-1.45502228044773,-1.38923460267853,
-1.3265205751834,-1.26669886884287,-1.20909993484359,-1.15227786115506,
-1.09526869988759,-1.03807287674761,-0.979856117355335,-0.917508293433697,
-0.851705632256396,-0.782466326919254,-0.709863093111388,-0.634726037442554,
-0.555385282762235,-0.481050928781323,-0.403338688398482,-0.320930918924746,
-0.234066753872441,-0.147080803661418,-0.0621010514640444,0.),
 .UNSPECIFIED.);
#108=B_SPLINE_CURVE_WITH_KNOTS('',3,(#10782,#10783,#10784,#10785,#10786,
#10787,#10788,#10789,#10790,#10791,#10792,#10793),.UNSPECIFIED.,.F.,.F.,
(4,2,2,2,2,4),(-8.5482923307436,-7.74150904834439,-6.97394683763538,-6.20677862322595,
-5.20801064419706,-3.86462956150548),.UNSPECIFIED.);
#109=B_SPLINE_CURVE_WITH_KNOTS('',3,(#10841,#10842,#10843,#10844,#10845,
#10846,#10847,#10848),.UNSPECIFIED.,.F.,.F.,(4,2,2,4),(0.000486150394328964,
0.250000004296481,0.436057375062024,0.485741739397154),.UNSPECIFIED.);
#110=B_SPLINE_CURVE_WITH_KNOTS('',3,(#10852,#10853,#10854,#10855,#10856,
#10857,#10858,#10859),.UNSPECIFIED.,.F.,.F.,(4,2,2,4),(-0.485741739388686,
-0.436057375062167,-0.250000004296568,-0.000486150394336471),
 .UNSPECIFIED.);
#111=B_SPLINE_CURVE_WITH_KNOTS('',3,(#10860,#10861,#10862,#10863,#10864,
#10865,#10866,#10867,#10868,#10869,#10870,#10871),.UNSPECIFIED.,.F.,.F.,
(4,2,2,2,2,4),(-1.,-0.911417181577934,-0.82714074028049,-0.742907558806875,
-0.633245293286218,-0.485745357261071),.UNSPECIFIED.);
#112=B_SPLINE_CURVE_WITH_KNOTS('',3,(#10944,#10945,#10946,#10947,#10948,
#10949,#10950,#10951,#10952,#10953,#10954,#10955,#10956,#10957,#10958,#10959,
#10960,#10961,#10962,#10963,#10964,#10965,#10966,#10967,#10968,#10969,#10970,
#10971,#10972,#10973,#10974,#10975,#10976,#10977,#10978,#10979,#10980,#10981,
#10982,#10983,#10984,#10985,#10986,#10987,#10988,#10989,#10990,#10991,#10992,
#10993,#10994,#10995,#10996,#10997,#10998,#10999,#11000,#11001,#11002,#11003,
#11004,#11005,#11006,#11007,#11008,#11009,#11010,#11011,#11012,#11013,#11014,
#11015,#11016,#11017,#11018,#11019,#11020,#11021,#11022,#11023,#11024,#11025,
#11026,#11027,#11028,#11029,#11030,#11031,#11032,#11033,#11034,#11035,#11036,
#11037,#11038,#11039,#11040,#11041,#11042,#11043,#11044,#11045,#11046),
 .UNSPECIFIED.,.F.,.F.,(4,3,3,3,3,3,3,3,3,3,3,3,3,3,3,3,3,3,3,3,3,3,3,3,
3,3,3,3,3,3,3,3,3,3,4),(10.3765483376485,10.4759402027806,10.5793082825219,
10.6784508692425,10.7775387594599,10.8766044822859,10.9756805342132,11.0748594189434,
11.1740994295162,11.2734971320225,11.3028848407106,11.4035366366706,11.5040458940526,
11.604441769589,11.7047757700553,11.8050789264824,11.9053822307961,12.0057869498693,
12.1062407367629,12.2068773510693,12.3013539368137,12.401784255105,12.5020682067574,
12.6022340752359,12.7023353147295,12.8024032837535,12.9024692992144,13.0026350854369,
13.102848654931,13.2032457178991,13.2998230329169,13.4003060369769,13.500661779787,
13.6009053515717,13.6618569927778),.UNSPECIFIED.);
#113=B_SPLINE_CURVE_WITH_KNOTS('',3,(#11049,#11050,#11051,#11052,#11053,
#11054,#11055,#11056,#11057,#11058,#11059,#11060,#11061,#11062,#11063,#11064,
#11065,#11066,#11067,#11068,#11069,#11070,#11071,#11072,#11073,#11074,#11075,
#11076,#11077,#11078,#11079,#11080,#11081,#11082,#11083,#11084,#11085,#11086,
#11087,#11088,#11089,#11090,#11091,#11092,#11093,#11094,#11095,#11096,#11097,
#11098,#11099,#11100,#11101,#11102,#11103,#11104,#11105,#11106,#11107,#11108,
#11109,#11110),.UNSPECIFIED.,.F.,.F.,(4,2,2,2,2,2,2,2,2,2,2,2,2,2,2,2,2,
2,2,2,2,2,2,2,2,2,2,2,2,2,4),(-2.46836400305217,-2.46588308991174,-2.46291917044417,
-2.45431065559104,-2.40639634652271,-2.37549128637183,-2.36524340856034,
-2.35781521258133,-2.34987427534677,-2.33687237436732,-2.28350253421887,
-2.25546994759335,-2.23986353138549,-2.23429474379311,-2.23045748204932,
-2.2261999437853,-2.21834822932595,-2.18055988226961,-2.14842269765427,
-2.12834892767817,-2.11983491881741,-2.11336504532106,-2.10622759505867,
-2.09412995748809,-2.03544976313569,-2.0132907412493,-1.99999034003753,
-1.99491712618401,-1.99124091634937,-1.98688475739941,-1.98168879881574),
 .UNSPECIFIED.);
#114=B_SPLINE_CURVE_WITH_KNOTS('',3,(#11116,#11117,#11118,#11119,#11120,
#11121,#11122,#11123,#11124,#11125,#11126,#11127,#11128,#11129,#11130,#11131,
#11132,#11133,#11134,#11135,#11136,#11137,#11138,#11139,#11140,#11141,#11142,
#11143,#11144,#11145,#11146,#11147,#11148,#11149,#11150,#11151,#11152,#11153,
#11154,#11155,#11156,#11157,#11158,#11159,#11160,#11161,#11162,#11163,#11164,
#11165,#11166,#11167,#11168,#11169,#11170,#11171,#11172,#11173,#11174,#11175,
#11176,#11177,#11178,#11179,#11180,#11181,#11182,#11183,#11184,#11185,#11186,
#11187,#11188,#11189,#11190,#11191,#11192,#11193,#11194,#11195,#11196,#11197,
#11198,#11199,#11200,#11201,#11202,#11203,#11204,#11205,#11206,#11207,#11208,
#11209,#11210,#11211,#11212,#11213,#11214,#11215,#11216,#11217,#11218,#11219,
#11220,#11221,#11222,#11223,#11224,#11225,#11226,#11227,#11228,#11229,#11230,
#11231,#11232,#11233,#11234,#11235,#11236,#11237,#11238,#11239,#11240,#11241),
 .UNSPECIFIED.,.F.,.F.,(4,2,2,2,2,2,2,2,2,2,2,2,2,2,2,2,2,2,2,2,2,2,2,2,
2,2,2,2,2,2,2,2,2,2,2,2,2,2,2,2,2,2,2,2,2,2,2,2,2,2,2,2,2,2,2,2,2,2,2,2,
2,2,4),(-1.00835904403323,-0.99080432518265,-0.979541237995393,-0.972419892514247,
-0.965629640897204,-0.956134910559768,-0.929577207527792,-0.87178313919011,
-0.860189047875725,-0.855600929406102,-0.851788747324675,-0.847415298956124,
-0.839155061266686,-0.80725024107116,-0.7536374572217,-0.742212215530873,
-0.73505894663375,-0.72828590554082,-0.718894415834214,-0.693305032052475,
-0.641545231070419,-0.624464424244031,-0.618620970061326,-0.614781665995942,
-0.610591430736765,-0.603228446918461,-0.593773860243074,-0.570735343768825,
-0.51583731359318,-0.504582215938246,-0.497462389170024,-0.490671169066672,
-0.481171007479902,-0.45456102090177,-0.396384905750253,-0.385199575897539,
-0.380625843033889,-0.376816003063609,-0.37243098244482,-0.364116119529149,
-0.352980305291608,-0.321986540625464,-0.280059878532716,-0.267946611621798,
-0.260655272635707,-0.253936992395149,-0.24491300455158,-0.222417392301592,
-0.18370927488101,-0.153741583092926,-0.145772864692122,-0.141411447447901,
-0.137597295400466,-0.132133015536881,-0.11702265733268,-0.0897952434469178,
-0.0736061524808066,-0.0388048341471226,-0.0285900550703762,-0.0223642361463906,
-0.0160654146575395,-0.00877331750423353,-0.000703244481836463),
 .UNSPECIFIED.);
#115=B_SPLINE_CURVE_WITH_KNOTS('',3,(#11242,#11243,#11244,#11245,#11246,
#11247,#11248,#11249,#11250,#11251,#11252,#11253,#11254,#11255,#11256,#11257,
#11258,#11259,#11260,#11261,#11262,#11263,#11264,#11265,#11266,#11267,#11268,
#11269,#11270,#11271,#11272,#11273,#11274,#11275,#11276,#11277,#11278,#11279,
#11280,#11281,#11282,#11283,#11284,#11285,#11286,#11287,#11288,#11289,#11290,
#11291,#11292,#11293,#11294,#11295,#11296,#11297,#11298,#11299,#11300,#11301,
#11302,#11303,#11304,#11305),.UNSPECIFIED.,.F.,.F.,(4,3,3,3,3,3,3,3,3,3,
3,3,3,3,3,3,3,3,3,3,3,4),(13.6618569927778,13.7620143384374,13.8621578175854,
13.9623186264353,14.0625906318973,14.1629275590632,14.2634284535134,14.29829212902,
14.3988099483912,14.4991826767506,14.5994388277011,14.6996312262565,14.7997911050727,
14.8999496560058,15.0002083164209,15.1005150980094,15.2010048401475,15.2967612251232,
15.4075012668598,15.5179191901853,15.6277924052815,15.7079632676322),
 .UNSPECIFIED.);
#116=B_SPLINE_CURVE_WITH_KNOTS('',3,(#11306,#11307,#11308,#11309,#11310,
#11311,#11312,#11313,#11314,#11315,#11316,#11317,#11318,#11319,#11320,#11321,
#11322,#11323,#11324,#11325,#11326,#11327,#11328,#11329,#11330,#11331,#11332,
#11333,#11334,#11335,#11336,#11337,#11338,#11339,#11340,#11341,#11342,#11343,
#11344,#11345,#11346,#11347,#11348,#11349,#11350,#11351,#11352,#11353,#11354,
#11355,#11356,#11357,#11358,#11359,#11360,#11361,#11362,#11363,#11364,#11365,
#11366,#11367,#11368,#11369,#11370,#11371,#11372,#11373,#11374,#11375,#11376,
#11377,#11378,#11379,#11380,#11381,#11382,#11383,#11384,#11385,#11386,#11387,
#11388,#11389,#11390,#11391,#11392,#11393,#11394,#11395,#11396,#11397,#11398,
#11399,#11400,#11401,#11402,#11403,#11404,#11405,#11406,#11407,#11408,#11409,
#11410,#11411,#11412,#11413,#11414,#11415,#11416,#11417,#11418,#11419,#11420,
#11421,#11422,#11423,#11424,#11425,#11426,#11427,#11428,#11429,#11430,#11431,
#11432,#11433,#11434,#11435,#11436,#11437,#11438,#11439,#11440,#11441,#11442,
#11443,#11444,#11445,#11446,#11447,#11448,#11449,#11450,#11451,#11452,#11453,
#11454,#11455,#11456,#11457,#11458,#11459,#11460,#11461,#11462,#11463,#11464,
#11465,#11466,#11467,#11468,#11469,#11470,#11471,#11472,#11473,#11474,#11475,
#11476,#11477),.UNSPECIFIED.,.F.,.F.,(4,2,2,2,2,2,2,2,2,2,2,2,2,2,2,2,2,
2,2,2,2,2,2,2,2,2,2,2,2,2,2,2,2,2,2,2,2,2,2,2,2,2,2,2,2,2,2,2,2,2,2,2,2,
2,2,2,2,2,2,2,2,2,2,2,2,2,2,2,2,2,2,2,2,2,2,2,2,2,2,2,2,2,2,2,2,4),(-1.98168879881574,
-1.97887615210958,-1.94763859892647,-1.91750028502234,-1.88895906587764,
-1.87922652020951,-1.87235989604258,-1.86607996514539,-1.85573719076576,
-1.81805038466509,-1.78930140312251,-1.76614687342023,-1.75988880532066,
-1.75589178010414,-1.7522609105256,-1.74576379723582,-1.71987712175649,
-1.67618535909901,-1.65232774742581,-1.64310538004146,-1.63632804398489,
-1.62905260467462,-1.61715236703276,-1.5584603952577,-1.529325622837,-1.52277530992381,
-1.51874396018361,-1.51473777456654,-1.50821172613658,-1.48084211855695,
-1.43823205474181,-1.41467185768912,-1.40553887080573,-1.39882989395385,
-1.39163476591018,-1.37989475655699,-1.32871001506904,-1.30350811173531,
-1.28907094117812,-1.28370631444398,-1.27991598457261,-1.27552160878638,
-1.2673955578436,-1.23470780118329,-1.18199872995672,-1.17044704656154,
-1.16326329378536,-1.15649326887355,-1.14715711654298,-1.12210693026197,
-1.07305330407891,-1.05330481821552,-1.04720582269474,-1.04366311903891,
-1.03965334388989,-1.03315660382362,-1.00491522444594,-0.944741791267324,
-0.933175037625585,-0.925990866835437,-0.919226630282932,-0.909909304104162,
-0.885015947841081,-0.836829692081973,-0.815988396769207,-0.809799160662296,
-0.806243751883766,-0.802263740017218,-0.79589476177324,-0.77019251672917,
-0.714439218864002,-0.698903405616671,-0.690865009860394,-0.684240285657257,
-0.676338717619893,-0.66103986211829,-0.640358067293166,-0.613034008915922,
-0.582012274920213,-0.574000962598554,-0.569632024595309,-0.565819837988581,
-0.560372936862727,-0.545416229054894,-0.518667185138567,-0.487365959345673),
 .UNSPECIFIED.);
#117=B_SPLINE_CURVE_WITH_KNOTS('',3,(#11482,#11483,#11484,#11485,#11486,
#11487,#11488,#11489,#11490,#11491,#11492,#11493,#11494,#11495,#11496,#11497,
#11498,#11499,#11500,#11501,#11502,#11503,#11504,#11505,#11506,#11507,#11508,
#11509,#11510,#11511,#11512,#11513,#11514,#11515,#11516,#11517,#11518,#11519,
#11520,#11521,#11522,#11523,#11524,#11525,#11526,#11527,#11528,#11529,#11530,
#11531,#11532,#11533,#11534,#11535,#11536,#11537,#11538,#11539,#11540,#11541,
#11542,#11543,#11544,#11545,#11546,#11547,#11548,#11549,#11550,#11551,#11552,
#11553,#11554,#11555,#11556,#11557,#11558,#11559,#11560,#11561,#11562,#11563,
#11564,#11565,#11566,#11567,#11568,#11569,#11570,#11571,#11572,#11573,#11574,
#11575,#11576,#11577,#11578,#11579,#11580,#11581,#11582,#11583,#11584,#11585,
#11586,#11587,#11588,#11589,#11590,#11591,#11592,#11593,#11594,#11595,#11596,
#11597,#11598,#11599,#11600,#11601,#11602,#11603,#11604,#11605,#11606,#11607,
#11608,#11609,#11610,#11611,#11612,#11613,#11614,#11615,#11616,#11617,#11618,
#11619,#11620,#11621,#11622,#11623,#11624,#11625,#11626,#11627,#11628,#11629,
#11630,#11631,#11632,#11633,#11634,#11635,#11636,#11637,#11638,#11639,#11640,
#11641,#11642,#11643,#11644,#11645,#11646,#11647,#11648,#11649,#11650,#11651,
#11652,#11653),.UNSPECIFIED.,.F.,.F.,(4,2,2,2,2,2,2,2,2,2,2,2,2,2,2,2,2,
2,2,2,2,2,2,2,2,2,2,2,2,2,2,2,2,2,2,2,2,2,2,2,2,2,2,2,2,2,2,2,2,2,2,2,2,
2,2,2,2,2,2,2,2,2,2,2,2,2,2,2,2,2,2,2,2,2,2,2,2,2,2,2,2,2,2,2,2,4),(-2.50248360392367,
-2.47407561568409,-2.43362224671165,-2.4106280150226,-2.40154232941611,
-2.39481673446982,-2.38755375233706,-2.37557629553376,-2.3274062717911,
-2.3006792603101,-2.28573081645583,-2.28028540735249,-2.27647339985178,
-2.27210190428346,-2.26408344307706,-2.23289114242665,-2.20312962726049,
-2.18392479930568,-2.16939974687355,-2.16164016004058,-2.15500739766369,
-2.14679799246234,-2.13366875304952,-2.07151403352715,-2.05672046938795,
-2.04652322403861,-2.04178596083641,-2.03802492531491,-2.03320405588648,
-2.02221873139686,-1.96346721147729,-1.93678737955585,-1.92728100569733,
-1.92048916122654,-1.91337198159745,-1.90212849778767,-1.84034195318542,
-1.81294625323171,-1.80649006407928,-1.80249113989479,-1.79845968512279,
-1.79184989845132,-1.76109069764411,-1.72111621940969,-1.69825538472261,
-1.68918569231159,-1.68246165023475,-1.67519069576965,-1.66317669953361,
-1.61558779393993,-1.5884891746718,-1.57341967181971,-1.56795870060941,
-1.56414404436843,-1.5597793596647,-1.55179473981675,-1.52137287980442,
-1.49522843980624,-1.46340422692845,-1.4532421942805,-1.44702344661142,
-1.44019064912493,-1.43044738461142,-1.40129855057202,-1.37210882441159,
-1.34110042213582,-1.33308932327228,-1.32871902116904,-1.32490586816934,
-1.31945606037215,-1.30447545475975,-1.2776517604171,-1.22967939510834,
-1.2176914828043,-1.2104256852885,-1.20369963412152,-1.19461672140066,-1.17165495127793,
-1.1313311826467,-1.10099204653433,-1.09438311962162,-1.09035179644238,
-1.08635237010884,-1.07989470399861,-1.05245728926926,-1.00835904403323),
 .UNSPECIFIED.);
#118=B_SPLINE_CURVE_WITH_KNOTS('',3,(#11655,#11656,#11657,#11658,#11659,
#11660,#11661,#11662,#11663,#11664,#11665,#11666,#11667,#11668,#11669,#11670,
#11671,#11672,#11673,#11674,#11675,#11676,#11677,#11678,#11679,#11680,#11681,
#11682,#11683,#11684,#11685,#11686,#11687,#11688,#11689,#11690,#11691,#11692,
#11693,#11694,#11695,#11696,#11697,#11698,#11699,#11700,#11701,#11702,#11703,
#11704,#11705,#11706,#11707,#11708,#11709,#11710),.UNSPECIFIED.,.F.,.F.,
(4,2,2,2,2,2,2,2,2,2,2,2,2,2,2,2,2,2,2,2,2,2,2,2,2,2,2,4),(-0.487365959345673,
-0.470564312664979,-0.45858267467034,-0.451317489371573,-0.444589955523596,
-0.435501767533371,-0.412503106109016,-0.372045361245167,-0.341899322545666,
-0.335291466812455,-0.33125982565294,-0.327259600048952,-0.320798823614071,
-0.293300890879341,-0.231752022206382,-0.220465684395158,-0.213339615594384,
-0.206551694911002,-0.197071738340952,-0.170658718302693,-0.113888329504335,
-0.101497710838403,-0.0967566905152996,-0.0929500858939294,-0.0886871136675097,
-0.0809723696866922,-0.0359502418557884,-0.000724551695920961),
 .UNSPECIFIED.);
#119=B_SPLINE_CURVE_WITH_KNOTS('',3,(#11711,#11712,#11713,#11714,#11715,
#11716,#11717,#11718,#11719,#11720,#11721,#11722,#11723,#11724,#11725,#11726,
#11727,#11728,#11729,#11730,#11731,#11732,#11733,#11734,#11735,#11736,#11737,
#11738,#11739,#11740,#11741,#11742,#11743,#11744,#11745,#11746,#11747,#11748,
#11749,#11750,#11751,#11752,#11753,#11754,#11755,#11756,#11757,#11758,#11759,
#11760,#11761,#11762,#11763,#11764,#11765,#11766,#11767,#11768,#11769,#11770,
#11771,#11772,#11773,#11774,#11775,#11776,#11777,#11778,#11779,#11780,#11781,
#11782,#11783,#11784,#11785,#11786,#11787,#11788,#11789,#11790,#11791,#11792,
#11793,#11794,#11795,#11796,#11797,#11798,#11799,#11800,#11801,#11802,#11803,
#11804,#11805,#11806,#11807,#11808,#11809,#11810,#11811,#11812,#11813,#11814,
#11815,#11816,#11817,#11818,#11819,#11820,#11821,#11822,#11823,#11824,#11825,
#11826,#11827,#11828,#11829,#11830,#11831,#11832,#11833,#11834,#11835,#11836,
#11837,#11838,#11839,#11840),.UNSPECIFIED.,.F.,.F.,(4,3,3,3,3,3,3,3,3,3,
3,3,3,3,3,3,3,3,3,3,3,3,3,3,3,3,3,3,3,3,3,3,3,3,3,3,3,3,3,3,3,3,3,4),(21.9911485751284,
22.0924387715178,22.193756115275,22.2952120703206,22.3967363325759,22.4984725473193,
22.598192904953,22.6986966926657,22.7990551040477,22.8992965748876,22.9994740790185,
23.099618869796,23.1997621595773,23.3000053923226,23.4002966302333,23.5007708150454,
23.5966620010561,23.6971657361334,23.7975240967797,23.8977655200214,23.9979429784857,
24.0980877255971,24.1982309737833,24.2984741685247,24.3987653703273,24.4992395227271,
24.5951310971593,24.6956346239705,24.7959927721852,24.8962339777079,24.9964112153343,
25.0965557387948,25.1966987608204,25.2969417270206,25.3972326986099,25.4977066206725,
25.5936001932624,25.6940877321455,25.7944386585383,25.8946844403876,25.9948602026975,
26.0949960613067,26.1951428401909,26.2274452731783),.UNSPECIFIED.);
#120=B_SPLINE_CURVE_WITH_KNOTS('',3,(#11846,#11847,#11848,#11849,#11850,
#11851,#11852,#11853,#11854,#11855,#11856,#11857,#11858,#11859,#11860,#11861,
#11862,#11863,#11864,#11865,#11866,#11867,#11868,#11869,#11870,#11871,#11872,
#11873,#11874,#11875,#11876,#11877,#11878,#11879,#11880,#11881,#11882,#11883,
#11884,#11885,#11886,#11887,#11888,#11889,#11890,#11891,#11892,#11893,#11894,
#11895,#11896,#11897,#11898,#11899,#11900,#11901,#11902,#11903,#11904,#11905,
#11906,#11907,#11908,#11909,#11910,#11911,#11912,#11913,#11914,#11915,#11916,
#11917,#11918,#11919,#11920,#11921,#11922,#11923,#11924,#11925,#11926,#11927,
#11928,#11929,#11930,#11931,#11932,#11933,#11934,#11935,#11936,#11937,#11938,
#11939,#11940,#11941,#11942,#11943,#11944,#11945,#11946,#11947,#11948,#11949,
#11950,#11951,#11952,#11953,#11954,#11955,#11956,#11957,#11958,#11959,#11960,
#11961,#11962,#11963,#11964,#11965),.UNSPECIFIED.,.F.,.F.,(4,2,2,2,2,2,
2,2,2,2,2,2,2,2,2,2,2,2,2,2,2,2,2,2,2,2,2,2,2,2,2,2,2,2,2,2,2,2,2,2,2,2,
2,2,2,2,2,2,2,2,2,2,2,2,2,2,2,2,2,4),(-1.00820552373846,-0.994394655396467,
-0.964367093019684,-0.956397307792939,-0.95203611858455,-0.948221008334916,
-0.942754775052995,-0.92763777284904,-0.900387708944509,-0.853103222565575,
-0.841079094213585,-0.83380675407602,-0.827084341129394,-0.818021404607694,
-0.795210534269092,-0.755413229545206,-0.724369871629825,-0.717757876824139,
-0.713726280876762,-0.7097283157445,-0.703275582533351,-0.675927265057406,
-0.614119784339548,-0.602891872297349,-0.595778241935107,-0.588985391579343,
-0.579470252263594,-0.552704008992778,-0.493339080634471,-0.48281535532095,
-0.47802143504235,-0.474261734505149,-0.469419969764229,-0.458614928601644,
-0.442535892350851,-0.413359955945697,-0.37497716390833,-0.364580875422495,
-0.358322661255733,-0.351524983470061,-0.341984473236009,-0.314975535735101,
-0.253664521276312,-0.244603215148044,-0.240073462999185,-0.236294017156018,
-0.23112069660227,-0.218197636048589,-0.197143057470757,-0.140704394456143,
-0.128693347609297,-0.121422883457909,-0.114698405766845,-0.105626784261932,
-0.0827548282764922,-0.0489820852688783,-0.0148892268915053,-0.00679760338978686,
-0.0030868104747884,-0.000701448731005652),.UNSPECIFIED.);
#121=B_SPLINE_CURVE_WITH_KNOTS('',3,(#11966,#11967,#11968,#11969,#11970,
#11971,#11972,#11973,#11974,#11975,#11976,#11977,#11978,#11979,#11980,#11981,
#11982,#11983,#11984,#11985,#11986,#11987,#11988,#11989,#11990,#11991,#11992,
#11993,#11994,#11995,#11996,#11997,#11998,#11999,#12000,#12001,#12002,#12003,
#12004,#12005,#12006,#12007,#12008,#12009,#12010,#12011,#12012,#12013,#12014,
#12015,#12016,#12017,#12018,#12019,#12020,#12021,#12022,#12023,#12024,#12025,
#12026,#12027),.UNSPECIFIED.,.F.,.F.,(4,2,2,2,2,2,2,2,2,2,2,2,2,2,2,2,2,
2,2,2,2,2,2,2,2,2,2,2,2,2,4),(-2.98912631766799,-2.98751883418936,-2.98455840277561,
-2.97785124353937,-2.94286544624325,-2.90819033764507,-2.88541989426223,
-2.87636340785528,-2.86964277554806,-2.86236951039912,-2.85033711273869,
-2.79391604009925,-2.76533872074448,-2.75744477062747,-2.75314566555994,
-2.74931046315851,-2.74460825162245,-2.73259768601139,-2.67547941493075,
-2.64902807190514,-2.63954623204563,-2.63275918542872,-2.62563592466837,
-2.61435833120269,-2.55275128036213,-2.52526815635112,-2.51880862834569,
-2.51480937113557,-2.51077943238742,-2.50417504631604,-2.50248360392367),
 .UNSPECIFIED.);
#122=B_SPLINE_CURVE_WITH_KNOTS('',3,(#12029,#12030,#12031,#12032,#12033,
#12034,#12035,#12036,#12037,#12038,#12039,#12040,#12041,#12042,#12043,#12044,
#12045,#12046,#12047,#12048,#12049,#12050,#12051,#12052,#12053,#12054,#12055,
#12056,#12057,#12058,#12059,#12060,#12061,#12062,#12063,#12064,#12065,#12066,
#12067,#12068,#12069,#12070,#12071,#12072,#12073,#12074,#12075,#12076,#12077,
#12078,#12079,#12080,#12081,#12082,#12083,#12084,#12085,#12086,#12087,#12088,
#12089,#12090,#12091,#12092),.UNSPECIFIED.,.F.,.F.,(4,3,3,3,3,3,3,3,3,3,
3,3,3,3,3,3,3,3,3,3,3,4),(26.2274452731783,26.3277007622098,26.4280132896588,
26.5284985271382,26.5920692893656,26.6925729202986,26.7929311743964,26.8931724879587,
26.993349834888,27.0934944687626,27.1936376021625,27.2938806804709,27.3941717647521,
27.4946457991629,27.5905383854687,27.6906601857262,27.7906431130241,27.8905190749967,
27.9903298046759,28.0900991503633,28.1898994323691,28.2743338823081),
 .UNSPECIFIED.);
#123=B_SPLINE_CURVE_WITH_KNOTS('',3,(#12093,#12094,#12095,#12096,#12097,
#12098,#12099,#12100),.UNSPECIFIED.,.F.,.F.,(4,1,1,1,1,4),(28.2743397907761,
28.5890074815719,29.5874765776751,30.5859456737782,31.5844147698814,32.5105812343903),
 .UNSPECIFIED.);
#124=B_SPLINE_CURVE_WITH_KNOTS('',3,(#12105,#12106,#12107,#12108,#12109,
#12110,#12111,#12112,#12113,#12114,#12115,#12116,#12117,#12118,#12119,#12120,
#12121,#12122,#12123,#12124,#12125,#12126,#12127,#12128,#12129,#12130,#12131,
#12132,#12133,#12134,#12135,#12136,#12137,#12138,#12139,#12140,#12141,#12142,
#12143,#12144,#12145,#12146,#12147,#12148,#12149,#12150,#12151,#12152,#12153,
#12154,#12155,#12156,#12157,#12158,#12159,#12160,#12161,#12162,#12163,#12164,
#12165,#12166,#12167,#12168,#12169,#12170,#12171,#12172,#12173,#12174,#12175,
#12176,#12177,#12178,#12179,#12180,#12181,#12182,#12183,#12184,#12185,#12186,
#12187,#12188,#12189,#12190,#12191,#12192,#12193,#12194,#12195,#12196,#12197,
#12198,#12199,#12200,#12201,#12202,#12203,#12204,#12205,#12206,#12207,#12208,
#12209,#12210,#12211,#12212,#12213,#12214,#12215,#12216,#12217,#12218,#12219,
#12220,#12221,#12222,#12223,#12224,#12225,#12226,#12227,#12228,#12229,#12230,
#12231,#12232,#12233,#12234,#12235,#12236,#12237,#12238,#12239,#12240,#12241,
#12242,#12243,#12244,#12245,#12246,#12247,#12248,#12249,#12250,#12251,#12252,
#12253,#12254,#12255,#12256,#12257,#12258,#12259,#12260,#12261,#12262,#12263,
#12264,#12265,#12266,#12267,#12268,#12269,#12270,#12271,#12272,#12273,#12274,
#12275,#12276,#12277,#12278,#12279,#12280),.UNSPECIFIED.,.F.,.F.,(4,2,2,
2,2,2,2,2,2,2,2,2,2,2,2,2,2,2,2,2,2,2,2,2,2,2,2,2,2,2,2,2,2,2,2,2,2,2,2,
2,2,2,2,2,2,2,2,2,2,2,2,2,2,2,2,2,2,2,2,2,2,2,2,2,2,2,2,2,2,2,2,2,2,2,2,
2,2,2,2,2,2,2,2,2,2,2,2,4),(-2.50227618064395,-2.50221031618583,-2.49511085044294,
-2.48838692323815,-2.47888098188334,-2.45415586689061,-2.45019422125873,
-2.39343165660622,-2.38243550829324,-2.37756186823823,-2.3738018866163,
-2.36903869793777,-2.3586916698933,-2.299140410664,-2.27235801894746,-2.26284180697172,
-2.25604882269738,-2.2489355661288,-2.23770951543795,-2.17585070840769,
-2.1484991948045,-2.14204557028241,-2.13804744023506,-2.13401595230376,
-2.12740478230582,-2.09625875089389,-2.05657381629794,-2.03379677424679,
-2.02473833428267,-2.01801644152752,-2.01074199026837,-1.998708063534,-1.95153972463943,
-1.92417756707742,-1.90902432058123,-1.90355335493176,-1.89973753583041,
-1.89537843826185,-1.88741900518663,-1.85763986376304,-1.81960101048182,
-1.79650307208403,-1.78740416934828,-1.78067648104849,-1.77341842257003,
-1.76146641508434,-1.71291183047518,-1.6864186691951,-1.67154640110459,
-1.66611042521617,-1.6622996595805,-1.65792317141145,-1.64988151233805,
-1.61828237014342,-1.58913375317463,-1.56054141440432,-1.55084962126549,
-1.54402632659974,-1.53779870408895,-1.52758149042831,-1.49464976787876,
-1.46662609649144,-1.43662311742018,-1.43001821341247,-1.4259881298695,
-1.42198877001731,-1.41552935017593,-1.38803673181588,-1.32650028384284,
-1.31521592394445,-1.30809112628313,-1.30130441968337,-1.29182613694663,
-1.26541683649065,-1.20864233642671,-1.19627393349039,-1.19153492520049,
-1.18772915185835,-1.1834658078535,-1.17574790073308,-1.13187886395141,
-1.09065937512701,-1.07854685912919,-1.07125705935137,-1.06454097600566,
-1.05552123687758,-1.03304537697851,-1.00820552373846),.UNSPECIFIED.);
#125=B_SPLINE_CURVE_WITH_KNOTS('',3,(#12282,#12283,#12284,#12285,#12286,
#12287),.UNSPECIFIED.,.F.,.F.,(4,1,1,4),(32.5105812343903,32.5828838659845,
33.5813529620877,34.5575158971517),.UNSPECIFIED.);
#126=B_SPLINE_CURVE_WITH_KNOTS('',3,(#12288,#12289,#12290,#12291,#12292,
#12293,#12294,#12295,#12296,#12297,#12298,#12299,#12300,#12301,#12302,#12303,
#12304,#12305,#12306,#12307,#12308,#12309,#12310,#12311,#12312,#12313,#12314,
#12315,#12316,#12317,#12318,#12319,#12320,#12321,#12322,#12323,#12324,#12325,
#12326,#12327,#12328,#12329,#12330,#12331,#12332,#12333,#12334,#12335,#12336,
#12337,#12338,#12339,#12340,#12341,#12342,#12343,#12344,#12345,#12346,#12347,
#12348,#12349,#12350,#12351,#12352,#12353,#12354,#12355,#12356,#12357,#12358,
#12359,#12360,#12361,#12362,#12363,#12364,#12365,#12366,#12367,#12368,#12369,
#12370,#12371,#12372,#12373,#12374,#12375,#12376,#12377,#12378,#12379,#12380,
#12381,#12382,#12383,#12384,#12385,#12386,#12387,#12388,#12389,#12390,#12391,
#12392,#12393,#12394,#12395,#12396,#12397,#12398,#12399,#12400,#12401,#12402,
#12403,#12404,#12405,#12406,#12407,#12408,#12409,#12410,#12411,#12412,#12413,
#12414,#12415,#12416,#12417,#12418,#12419,#12420,#12421),.UNSPECIFIED.,
 .F.,.F.,(4,2,2,2,2,2,2,2,2,2,2,2,2,2,2,2,2,2,2,2,2,2,2,2,2,2,2,2,2,2,2,
2,2,2,2,2,2,2,2,2,2,2,2,2,2,2,2,2,2,2,2,2,2,2,2,2,2,2,2,2,2,2,2,2,2,2,4),
(-2.98897146095825,-2.98680475232993,-2.98409231131325,-2.98026226214111,
-2.97452190165697,-2.95716116705099,-2.94078050496096,-2.94044016274882,
-2.94005081874297,-2.93960561978467,-2.93909679028486,-2.9157730436606,
-2.88185404587531,-2.87175045709343,-2.86485335052196,-2.85788709311,-2.84741594372294,
-2.80708950807851,-2.77238891293047,-2.75515336956069,-2.74944451178113,
-2.74559095123431,-2.74133712717431,-2.73366532113475,-2.69050030949775,
-2.66036552013097,-2.64683517615848,-2.6355905460972,-2.62847346753744,
-2.62175848489122,-2.61230914645226,-2.58817957147445,-2.58289050051513,
-2.53768979135037,-2.51822047228037,-2.51229363190855,-2.50840099718553,
-2.50422623847947,-2.4969352788314,-2.45006955833457,-2.40925058339837,
-2.39808685366484,-2.39098594421377,-2.3842626232963,-2.37476098691795,
-2.35008752542848,-2.34570132039808,-2.28919656736693,-2.27826620949104,
-2.27340346110922,-2.26964361913121,-2.26487013317789,-2.25446419911136,
-2.19498132596812,-2.16820617382707,-2.15869047903897,-2.1518974826795,
-2.14478390958373,-2.1335567581347,-2.07169372652836,-2.04433861218451,
-2.03788462421192,-2.03388636361375,-2.02985489347567,-2.02324406442263,
-1.99222806350273,-1.98152642259734),.UNSPECIFIED.);
#127=B_SPLINE_CURVE_WITH_KNOTS('',3,(#12427,#12428,#12429,#12430,#12431,
#12432,#12433,#12434,#12435,#12436,#12437,#12438,#12439,#12440,#12441,#12442,
#12443,#12444,#12445,#12446,#12447,#12448,#12449,#12450,#12451,#12452,#12453,
#12454,#12455,#12456,#12457,#12458,#12459,#12460,#12461,#12462,#12463,#12464,
#12465,#12466,#12467,#12468,#12469,#12470,#12471,#12472,#12473,#12474,#12475,
#12476,#12477,#12478,#12479,#12480,#12481,#12482,#12483,#12484,#12485,#12486,
#12487,#12488,#12489,#12490,#12491,#12492,#12493,#12494,#12495,#12496,#12497,
#12498,#12499,#12500,#12501,#12502,#12503,#12504,#12505,#12506,#12507,#12508,
#12509,#12510,#12511,#12512,#12513,#12514,#12515,#12516,#12517,#12518,#12519,
#12520,#12521,#12522,#12523,#12524,#12525,#12526,#12527,#12528,#12529,#12530,
#12531,#12532,#12533,#12534,#12535,#12536,#12537,#12538,#12539,#12540,#12541,
#12542),.UNSPECIFIED.,.F.,.F.,(4,2,2,2,2,2,2,2,2,2,2,2,2,2,2,2,2,2,2,2,
2,2,2,2,2,2,2,2,2,2,2,2,2,2,2,2,2,2,2,2,2,2,2,2,2,2,2,2,2,2,2,2,2,2,2,2,
2,4),(-1.00824895752189,-0.978795587655649,-0.973940169113513,-0.966704674974702,
-0.945174696752521,-0.93700967812232,-0.93025151137541,-0.923204056888826,
-0.91231847285143,-0.867841797615394,-0.824672539001548,-0.816995293844911,
-0.81273966388343,-0.808885312912722,-0.803176532559376,-0.785949046709813,
-0.751281937183289,-0.710926412153754,-0.700464721990181,-0.693498916050672,
-0.686597762763197,-0.676479896001568,-0.642383387295629,-0.598315198314666,
-0.583204394967097,-0.577592764607878,-0.573754519597351,-0.569458441085479,
-0.561584170030399,-0.533188963403702,-0.477360969638919,-0.464899553471184,
-0.457539130815347,-0.450842460305814,-0.441975954589279,-0.420658870141396,
-0.385677852086332,-0.350670892870582,-0.342538469709235,-0.338142265526879,
-0.334335627842033,-0.328934779346477,-0.314344315452468,-0.288702819073133,
-0.23873941513685,-0.226903572456554,-0.219667610225886,-0.212929340436927,
-0.203767220144369,-0.180172333038482,-0.137508455793972,-0.110186082098065,
-0.103649432251847,-0.09963317306983,-0.0956184774177959,-0.0890894222704663,
-0.0599963915802122,-0.000701990655493575),.UNSPECIFIED.);
#128=B_SPLINE_CURVE_WITH_KNOTS('',3,(#12543,#12544,#12545,#12546,#12547,
#12548,#12549,#12550,#12551,#12552,#12553,#12554,#12555,#12556,#12557,#12558,
#12559,#12560,#12561,#12562,#12563,#12564,#12565,#12566,#12567,#12568,#12569,
#12570,#12571,#12572,#12573,#12574,#12575,#12576,#12577,#12578,#12579,#12580,
#12581,#12582,#12583,#12584,#12585,#12586,#12587,#12588,#12589,#12590,#12591,
#12592,#12593,#12594,#12595,#12596,#12597,#12598,#12599,#12600,#12601,#12602,
#12603,#12604),.UNSPECIFIED.,.F.,.F.,(4,2,2,2,2,2,2,2,2,2,2,2,2,2,2,2,2,
2,2,2,2,2,2,2,2,2,2,2,2,2,4),(-2.9889610906993,-2.98169081755074,-2.97482435504751,
-2.96852395308731,-2.96229608080387,-2.95207870536583,-2.91726567422965,
-2.89846756409784,-2.8730710264003,-2.85856467034494,-2.8531752531943,-2.84937088471838,
-2.84497016143403,-2.83681363613837,-2.7743969501821,-2.7472719564497,-2.73772111086022,
-2.73092228619588,-2.72466711190907,-2.71428595266541,-2.67610581457717,
-2.63961713915945,-2.62194583976429,-2.61619183344614,-2.61233062219264,
-2.60809464247292,-2.60050865558634,-2.55632933181388,-2.52675714512438,
-2.51336724670804,-2.50227618064395),.UNSPECIFIED.);
#129=B_SPLINE_CURVE_WITH_KNOTS('',3,(#12605,#12606,#12607,#12608,#12609,
#12610,#12611,#12612,#12613,#12614,#12615,#12616,#12617,#12618,#12619,#12620,
#12621,#12622,#12623,#12624,#12625,#12626,#12627,#12628,#12629,#12630,#12631,
#12632,#12633,#12634,#12635,#12636,#12637,#12638,#12639,#12640,#12641,#12642,
#12643,#12644,#12645,#12646,#12647,#12648,#12649,#12650,#12651,#12652,#12653,
#12654,#12655,#12656,#12657,#12658,#12659,#12660,#12661,#12662,#12663,#12664,
#12665,#12666,#12667,#12668,#12669,#12670,#12671,#12672,#12673,#12674,#12675,
#12676,#12677,#12678,#12679,#12680,#12681,#12682,#12683,#12684,#12685,#12686,
#12687,#12688,#12689,#12690,#12691,#12692,#12693,#12694,#12695,#12696,#12697,
#12698,#12699,#12700,#12701,#12702,#12703,#12704,#12705,#12706,#12707,#12708,
#12709,#12710,#12711,#12712,#12713,#12714,#12715,#12716,#12717,#12718,#12719,
#12720,#12721,#12722,#12723,#12724,#12725,#12726,#12727,#12728,#12729,#12730,
#12731,#12732,#12733,#12734,#12735,#12736,#12737,#12738,#12739,#12740,#12741,
#12742,#12743,#12744,#12745,#12746,#12747,#12748,#12749,#12750,#12751,#12752,
#12753,#12754,#12755,#12756,#12757,#12758,#12759,#12760,#12761,#12762,#12763,
#12764,#12765,#12766,#12767,#12768,#12769,#12770,#12771,#12772,#12773,#12774,
#12775,#12776,#12777,#12778,#12779,#12780),.UNSPECIFIED.,.F.,.F.,(4,2,2,
2,2,2,2,2,2,2,2,2,2,2,2,2,2,2,2,2,2,2,2,2,2,2,2,2,2,2,2,2,2,2,2,2,2,2,2,
2,2,2,2,2,2,2,2,2,2,2,2,2,2,2,2,2,2,2,2,2,2,2,2,2,2,2,2,2,2,2,2,2,2,2,2,
2,2,2,2,2,2,2,2,2,2,2,2,4),(-1.98152642259734,-1.95244157766786,-1.92963461939331,
-1.92057219071929,-1.91384962433673,-1.90657662092182,-1.89455046241958,
-1.84720247251783,-1.81995006589501,-1.8048314609841,-1.79936466760284,
-1.7955493995533,-1.79118817423857,-1.78321899257226,-1.75318846779628,
-1.71457028264026,-1.69210445501782,-1.68308590132271,-1.6763696553837,
-1.66907869055357,-1.65696209223008,-1.61539805487165,-1.58408453932364,
-1.56774865696872,-1.56213809796925,-1.55830079296156,-1.55400606411838,
-1.54613499845678,-1.49509745297723,-1.45776168025704,-1.44741496758706,
-1.44116560817109,-1.43436175724332,-1.42478209254381,-1.39737502024553,
-1.36646285930353,-1.33509422145299,-1.3270655399389,-1.32269188956398,
-1.31888043228983,-1.31343942375725,-1.29852526984928,-1.27190382788032,
-1.22361058163178,-1.21164477923068,-1.20438411122893,-1.19765760916817,
-1.18856601883069,-1.16552854846227,-1.1276949671944,-1.09758961382633,
-1.08961651529104,-1.08525456388988,-1.08143959889417,-1.07597475536949,
-1.0608698118706,-1.03365869651685,-0.9863043273708,-0.974282737987403,
-0.967010801791594,-0.960288080398835,-0.95122370929373,-0.928402989711735,
-0.888574120991167,-0.857565200069573,-0.850953060173582,-0.846921378460218,
-0.842923378362021,-0.836470739668188,-0.809128628613734,-0.747298429882624,
-0.736073282028595,-0.728960099410305,-0.722166809630299,-0.712649634675957,
-0.685865629050649,-0.626374982746974,-0.61594420134626,-0.611166235284037,
-0.607406266658429,-0.602547753497168,-0.591643420466857,-0.535253948984027,
-0.530469855064616,-0.506035216613575,-0.496555676232774,-0.489835515447429,
-0.487400405256145),.UNSPECIFIED.);
#130=B_SPLINE_CURVE_WITH_KNOTS('',3,(#12785,#12786,#12787,#12788,#12789,
#12790,#12791,#12792,#12793,#12794,#12795,#12796,#12797,#12798,#12799,#12800,
#12801,#12802,#12803,#12804,#12805,#12806,#12807,#12808,#12809,#12810,#12811,
#12812,#12813,#12814,#12815,#12816,#12817,#12818,#12819,#12820,#12821,#12822,
#12823,#12824,#12825,#12826,#12827,#12828,#12829,#12830,#12831,#12832,#12833,
#12834,#12835,#12836,#12837,#12838,#12839,#12840,#12841,#12842,#12843,#12844,
#12845,#12846,#12847,#12848,#12849,#12850,#12851,#12852,#12853,#12854,#12855,
#12856,#12857,#12858,#12859,#12860,#12861,#12862,#12863,#12864,#12865,#12866,
#12867,#12868,#12869,#12870,#12871,#12872,#12873,#12874,#12875,#12876,#12877,
#12878,#12879,#12880,#12881,#12882,#12883,#12884,#12885,#12886,#12887,#12888,
#12889,#12890,#12891,#12892,#12893,#12894,#12895,#12896,#12897,#12898,#12899,
#12900,#12901,#12902,#12903,#12904,#12905,#12906,#12907,#12908,#12909,#12910,
#12911,#12912,#12913,#12914,#12915,#12916,#12917,#12918,#12919,#12920,#12921,
#12922,#12923,#12924,#12925,#12926,#12927,#12928,#12929,#12930,#12931,#12932,
#12933,#12934,#12935,#12936,#12937,#12938,#12939,#12940,#12941,#12942,#12943,
#12944,#12945,#12946,#12947,#12948,#12949,#12950,#12951,#12952,#12953,#12954,
#12955,#12956,#12957,#12958,#12959,#12960,#12961,#12962,#12963,#12964),
 .UNSPECIFIED.,.F.,.F.,(4,2,2,2,2,2,2,2,2,2,2,2,2,2,2,2,2,2,2,2,2,2,2,2,
2,2,2,2,2,2,2,2,2,2,2,2,2,2,2,2,2,2,2,2,2,2,2,2,2,2,2,2,2,2,2,2,2,2,2,2,
2,2,2,2,2,2,2,2,2,2,2,2,2,2,2,2,2,2,2,2,2,2,2,2,2,2,2,2,2,4),(-2.50223904448815,
-2.48458676113316,-2.47801768456686,-2.47399579738338,-2.46999039961284,
-2.46349942936955,-2.43714924866715,-2.39376260974356,-2.36999170754781,
-2.36081147857154,-2.35407294199949,-2.34684867933954,-2.3350605115819,
-2.28461561836689,-2.259239287865,-2.24924722624857,-2.2415749184917,-2.23732145384687,
-2.2335126908396,-2.22875832297729,-2.21888199985122,-2.16006375543227,
-2.13337966289093,-2.12387449951752,-2.11708412372897,-2.10996900842573,
-2.09872994063561,-2.03695034833215,-2.00956559254414,-2.00311117545505,
-1.99911326788349,-1.99508276237611,-1.98847440189447,-1.95768804202051,
-1.91774856834776,-1.89490047002733,-1.88583390262889,-1.87911163900697,
-1.87184210332913,-1.85982922941041,-1.80190931288493,-1.77454156250601,
-1.76678990618451,-1.7625197695934,-1.7587168541263,-1.75399040089237,-1.74177516473542,
-1.73034688350027,-1.68279669421211,-1.65805070817618,-1.64875458338047,
-1.6419971632621,-1.63481262276749,-1.62322843877648,-1.56311006788951,
-1.53480764040119,-1.52831133306707,-1.52430415051402,-1.52076970939507,
-1.51469218033872,-1.49505760547634,-1.44746378079865,-1.42145443285424,
-1.41179979094372,-1.40505046973743,-1.39799194662127,-1.38704595408075,
-1.37399162429497,-1.34573750542516,-1.29889194561219,-1.29159304919151,
-1.28741637886326,-1.28352409564388,-1.27760094847803,-1.25817374116419,
-1.2131921836749,-1.20672884800698,-1.18334970985123,-1.17398663189192,
-1.16721788917444,-1.16005469175799,-1.14858096152927,-1.10783532675572,
-1.06158033903093,-1.05421194259443,-1.05002054600416,-1.04613584139557,
-1.04025478538002,-1.02129088525616,-1.00824895752189),.UNSPECIFIED.);
#131=B_SPLINE_CURVE_WITH_KNOTS('',3,(#12966,#12967,#12968,#12969,#12970,
#12971,#12972,#12973,#12974,#12975,#12976,#12977,#12978,#12979,#12980,#12981,
#12982,#12983,#12984,#12985,#12986,#12987,#12988,#12989,#12990,#12991,#12992,
#12993,#12994,#12995,#12996,#12997,#12998,#12999,#13000,#13001,#13002,#13003,
#13004,#13005,#13006,#13007,#13008,#13009,#13010,#13011,#13012,#13013,#13014,
#13015,#13016,#13017,#13018,#13019,#13020,#13021,#13022,#13023,#13024,#13025,
#13026,#13027,#13028,#13029),.UNSPECIFIED.,.F.,.F.,(4,2,2,2,2,2,2,2,2,2,
2,2,2,2,2,2,2,2,2,2,2,2,2,2,2,2,2,2,2,2,2,4),(-0.487400405256145,-0.482727071494558,
-0.471527600046117,-0.458068493533978,-0.42822621030856,-0.384469184654347,
-0.37683819492679,-0.372592581288493,-0.368734932123639,-0.363003859966925,
-0.345557701741069,-0.310003822371837,-0.270911176796646,-0.260405860468918,
-0.253432618394381,-0.246540393641908,-0.236465943941031,-0.20302172959381,
-0.174759519540837,-0.14516598005652,-0.138565888098001,-0.134536618828129,
-0.13053592609133,-0.124071145062031,-0.0964725702842965,-0.0702072811410385,
-0.0488732556113054,-0.0294385074583665,-0.0207592877466262,-0.0142496064044319,
-0.00745404941009283,-0.000701089417020961),.UNSPECIFIED.);
#132=B_SPLINE_CURVE_WITH_KNOTS('',3,(#13030,#13031,#13032,#13033,#13034,
#13035,#13036,#13037,#13038,#13039,#13040,#13041,#13042,#13043,#13044,#13045,
#13046,#13047,#13048,#13049,#13050,#13051,#13052,#13053,#13054,#13055,#13056,
#13057,#13058,#13059,#13060,#13061,#13062,#13063,#13064,#13065,#13066,#13067,
#13068,#13069,#13070,#13071,#13072,#13073,#13074,#13075,#13076,#13077,#13078,
#13079,#13080,#13081,#13082,#13083,#13084,#13085,#13086,#13087,#13088,#13089,
#13090,#13091,#13092,#13093,#13094,#13095,#13096,#13097,#13098,#13099,#13100,
#13101,#13102,#13103,#13104,#13105,#13106,#13107,#13108,#13109,#13110,#13111,
#13112,#13113,#13114,#13115,#13116,#13117,#13118,#13119,#13120,#13121,#13122,
#13123,#13124,#13125,#13126,#13127,#13128,#13129,#13130,#13131,#13132,#13133,
#13134,#13135,#13136,#13137,#13138,#13139,#13140,#13141,#13142,#13143,#13144,
#13145),.UNSPECIFIED.,.F.,.F.,(4,2,2,2,2,2,2,2,2,2,2,2,2,2,2,2,2,2,2,2,
2,2,2,2,2,2,2,2,2,2,2,2,2,2,2,2,2,2,2,2,2,2,2,2,2,2,2,2,2,2,2,2,2,2,2,2,
2,4),(-2.98881319574078,-2.98092667063717,-2.91773801648977,-2.90229028970612,
-2.89178096031394,-2.88698970111545,-2.88360134363954,-2.87896353694705,
-2.86931929279196,-2.80884416450732,-2.78194543849523,-2.77241749892472,
-2.76562269829647,-2.7585132526015,-2.7473057944763,-2.68535417733898,-2.65804884168758,
-2.65159743128282,-2.64759983518693,-2.64356804408673,-2.63695512095839,
-2.60545508992586,-2.5660254796506,-2.54332177012797,-2.53427279780556,
-2.52755241270359,-2.52027442406673,-2.50822212404284,-2.46146920969877,
-2.43383328414512,-2.41859305924976,-2.41311148813477,-2.40929420224561,
-2.40494054174156,-2.39700638804516,-2.36791917182915,-2.32858257642323,
-2.30590602332798,-2.29686062427832,-2.290140835567,-2.28286155347665,-2.27080237774554,
-2.22423418412807,-2.19647729886502,-2.18119903840766,-2.17571287769436,
-2.17189496364491,-2.16754364149193,-2.15962028434921,-2.10943000586541,
-2.07430097796159,-2.06257364126141,-2.05536076730688,-2.04861603678536,
-2.03940062629956,-2.01710211576782,-2.00855411566961,-1.98138385324549),
 .UNSPECIFIED.);
#133=B_SPLINE_CURVE_WITH_KNOTS('',3,(#13151,#13152,#13153,#13154,#13155,
#13156,#13157,#13158),.UNSPECIFIED.,.F.,.F.,(4,1,1,1,1,4),(53.4070818023739,
54.2370559731461,55.2355250692492,56.2339941653524,57.2324632614555,57.6442142744167),
 .UNSPECIFIED.);
#134=B_SPLINE_CURVE_WITH_KNOTS('',3,(#13159,#13160,#13161,#13162,#13163,
#13164,#13165,#13166,#13167,#13168,#13169,#13170,#13171,#13172,#13173,#13174,
#13175,#13176,#13177,#13178,#13179,#13180,#13181,#13182,#13183,#13184,#13185,
#13186,#13187,#13188,#13189,#13190,#13191,#13192,#13193,#13194,#13195,#13196,
#13197,#13198,#13199,#13200,#13201,#13202,#13203,#13204,#13205,#13206,#13207,
#13208,#13209,#13210,#13211,#13212,#13213,#13214,#13215,#13216,#13217,#13218,
#13219,#13220,#13221,#13222),.UNSPECIFIED.,.F.,.F.,(4,2,2,2,2,2,2,2,2,2,
2,2,2,2,2,2,2,2,2,2,2,2,2,2,2,2,2,2,2,2,2,4),(-2.98851908576972,-2.95954428231633,
-2.95455224709358,-2.9508390566069,-2.9474336905644,-2.94296059961915,-2.93418670148345,
-2.89299194574678,-2.86155920997997,-2.86033142855133,-2.856013111439,-2.84636036089806,
-2.8364825166323,-2.82962843921203,-2.82261521908214,-2.81189060279604,
-2.75334077731679,-2.72440308382134,-2.71646874334363,-2.71216202486354,
-2.70833073623885,-2.70364384534931,-2.69173203180844,-2.64938273341975,
-2.62311596385264,-2.60516227090508,-2.59680265662696,-2.59022271380644,
-2.58260156877934,-2.56918037606721,-2.51480708332722,-2.50223904448815),
 .UNSPECIFIED.);
#135=B_SPLINE_CURVE_WITH_KNOTS('',3,(#13223,#13224,#13225,#13226,#13227,
#13228,#13229,#13230,#13231,#13232,#13233,#13234,#13235,#13236,#13237,#13238,
#13239,#13240,#13241,#13242,#13243,#13244,#13245,#13246,#13247,#13248,#13249,
#13250,#13251,#13252,#13253,#13254,#13255,#13256,#13257,#13258,#13259,#13260,
#13261,#13262,#13263,#13264,#13265,#13266,#13267,#13268,#13269,#13270,#13271,
#13272,#13273,#13274,#13275,#13276,#13277,#13278,#13279,#13280,#13281,#13282,
#13283,#13284,#13285,#13286,#13287,#13288,#13289,#13290,#13291,#13292,#13293,
#13294,#13295,#13296,#13297,#13298,#13299,#13300,#13301,#13302,#13303,#13304,
#13305,#13306,#13307,#13308,#13309,#13310,#13311,#13312,#13313,#13314,#13315,
#13316,#13317,#13318,#13319,#13320,#13321,#13322,#13323,#13324,#13325,#13326,
#13327,#13328,#13329,#13330,#13331,#13332,#13333,#13334,#13335,#13336,#13337,
#13338,#13339,#13340,#13341,#13342,#13343,#13344,#13345,#13346,#13347,#13348,
#13349,#13350,#13351,#13352,#13353,#13354,#13355,#13356,#13357,#13358,#13359,
#13360,#13361,#13362,#13363,#13364,#13365,#13366,#13367,#13368,#13369,#13370,
#13371,#13372,#13373,#13374,#13375,#13376,#13377,#13378,#13379,#13380,#13381,
#13382,#13383,#13384,#13385,#13386,#13387,#13388,#13389,#13390,#13391,#13392,
#13393,#13394,#13395,#13396,#13397,#13398,#13399,#13400),.UNSPECIFIED.,
 .F.,.F.,(4,2,2,2,2,2,2,2,2,2,2,2,2,2,2,2,2,2,2,2,2,2,2,2,2,2,2,2,2,2,2,
2,2,2,2,2,2,2,2,2,2,2,2,2,2,2,2,2,2,2,2,2,2,2,2,2,2,2,2,2,2,2,2,2,2,2,2,
2,2,2,2,2,2,2,2,2,2,2,2,2,2,2,2,2,2,2,2,2,4),(-1.98138385324549,-1.97081674774911,
-1.9456115031022,-1.93926934873765,-1.93529468115891,-1.9312378318781,-1.92450583382052,
-1.88725837866581,-1.85204981831191,-1.8306596161908,-1.82178498879674,
-1.81508884593133,-1.80773549980442,-1.79530299307739,-1.73493798628633,
-1.71685285639854,-1.70515227697233,-1.70016441332826,-1.69675925022926,
-1.69227524726658,-1.683450328206,-1.62185210143155,-1.59481934469136,-1.58527781096153,
-1.57848067581286,-1.57222376302594,-1.5618318534935,-1.5234865409652,-1.49454974399244,
-1.47081834938693,-1.46443489806573,-1.46084470323356,-1.45690518228799,
-1.45073603060133,-1.42823500353449,-1.37218900009806,-1.35430544979577,
-1.34595627659711,-1.33931539395311,-1.33166169327375,-1.31769264226281,
-1.28872018315684,-1.23726881319757,-1.22869734229427,-1.22426269971512,
-1.22046667708175,-1.21514026034268,-1.20111135939357,-1.17708927395995,
-1.12415994702007,-1.11265042717573,-1.1054808405156,-1.09871664157442,
-1.08937727067739,-1.06425345470384,-1.01491613517698,-0.995320747319436,
-0.989247653604348,-0.985714142538938,-0.981706116170247,-0.975205382501773,
-0.946776575961122,-0.886936276590112,-0.875304654848065,-0.868110874954834,
-0.861357978243554,-0.852089530397305,-0.827585822571833,-0.781153723671151,
-0.75834823461594,-0.752039233746843,-0.748462864296003,-0.744508571336025,
-0.738266620556866,-0.714699100119087,-0.685436100981927,-0.647033847847996,
-0.636636327204653,-0.630378203478102,-0.623581270756459,-0.614043093542911,
-0.587053645027215,-0.525906231617863,-0.516725698006973,-0.512173570137452,
-0.508397613106541,-0.503258511886453,-0.490568486782124,-0.487221889316969),
 .UNSPECIFIED.);
#136=B_SPLINE_CURVE_WITH_KNOTS('',3,(#13406,#13407,#13408,#13409,#13410,
#13411,#13412,#13413,#13414,#13415,#13416,#13417,#13418,#13419,#13420,#13421,
#13422,#13423,#13424,#13425,#13426,#13427,#13428,#13429,#13430,#13431,#13432,
#13433,#13434,#13435,#13436,#13437,#13438,#13439,#13440,#13441,#13442,#13443,
#13444,#13445,#13446,#13447,#13448,#13449,#13450,#13451,#13452,#13453,#13454,
#13455,#13456,#13457,#13458,#13459,#13460,#13461,#13462,#13463,#13464,#13465,
#13466,#13467,#13468,#13469,#13470,#13471,#13472,#13473,#13474,#13475,#13476,
#13477,#13478,#13479,#13480,#13481,#13482,#13483,#13484,#13485,#13486,#13487,
#13488,#13489,#13490,#13491,#13492,#13493,#13494,#13495,#13496,#13497,#13498,
#13499,#13500,#13501,#13502,#13503,#13504,#13505,#13506,#13507,#13508,#13509,
#13510,#13511,#13512,#13513,#13514,#13515,#13516,#13517,#13518,#13519,#13520,
#13521,#13522,#13523,#13524,#13525,#13526,#13527,#13528,#13529,#13530,#13531,
#13532,#13533,#13534,#13535),.UNSPECIFIED.,.F.,.F.,(4,3,3,3,3,3,3,3,3,3,
3,3,3,3,3,3,3,3,3,3,3,3,3,3,3,3,3,3,3,3,3,3,3,3,3,3,3,3,3,3,3,3,3,4),(59.690260418206,
59.7936358758742,59.9021945443469,60.0058912267106,60.1097115732471,60.2137481729558,
60.227870549765,60.3283743001658,60.4287326727968,60.5289741029433,60.6291515652241,
60.7292963130688,60.8294395589074,60.9296827464682,61.0299739384437,61.1304480766276,
61.2263396458681,61.3268434273722,61.427201833822,61.5274433016728,61.6276208039963,
61.7277655941466,61.8279088844805,61.9281521196312,62.0284433609616,62.1289175508793,
62.2248087419713,62.3253114183611,62.4256687161363,62.5259090751807,62.626085469101,
62.7262291527654,62.8263713400464,62.9266134853021,63.0269036421253,63.1273767696289,
63.2232778380744,63.3237600264403,63.4241074764649,63.5243516448779,63.6248681856545,
63.7250146750007,63.8257162414925,63.9264178079843),.UNSPECIFIED.);
#137=B_SPLINE_CURVE_WITH_KNOTS('',3,(#13536,#13537,#13538,#13539,#13540,
#13541),.UNSPECIFIED.,.F.,.F.,(4,1,1,4),(57.6442142744167,58.2309323575587,
59.2294014536618,59.6902576284875),.UNSPECIFIED.);
#138=B_SPLINE_CURVE_WITH_KNOTS('',3,(#13543,#13544,#13545,#13546,#13547,
#13548,#13549,#13550,#13551,#13552,#13553,#13554,#13555,#13556,#13557,#13558,
#13559,#13560,#13561,#13562,#13563,#13564,#13565,#13566,#13567,#13568,#13569,
#13570,#13571,#13572,#13573,#13574,#13575,#13576,#13577,#13578,#13579,#13580,
#13581,#13582,#13583,#13584,#13585,#13586,#13587,#13588,#13589,#13590,#13591,
#13592,#13593,#13594,#13595,#13596,#13597,#13598,#13599,#13600,#13601,#13602),
 .UNSPECIFIED.,.F.,.F.,(4,2,2,2,2,2,2,2,2,2,2,2,2,2,2,2,2,2,2,2,2,2,2,2,
2,2,2,2,2,4),(-0.487221889316969,-0.470103144983147,-0.416125571285123,
-0.402394763976587,-0.394708899705259,-0.38806972450983,-0.379761768066223,
-0.362136994090603,-0.336616220094698,-0.296396875014931,-0.281822048335411,
-0.276281493998449,-0.27245506965538,-0.268128720078924,-0.260102691018754,
-0.230367336116737,-0.173201352701178,-0.162268799704257,-0.155213065009728,
-0.148384337630516,-0.138661220765493,-0.10973105246942,-0.0542361797896722,
-0.0428673458297301,-0.0379842979785921,-0.0342207570513087,-0.0306022644981407,
-0.0259058737628287,-0.0168229950680565,-0.000700837973673536),
 .UNSPECIFIED.);
#139=B_SPLINE_CURVE_WITH_KNOTS('',3,(#13603,#13604,#13605,#13606,#13607,
#13608,#13609,#13610,#13611,#13612,#13613,#13614,#13615,#13616,#13617,#13618,
#13619,#13620,#13621,#13622,#13623,#13624,#13625,#13626,#13627,#13628,#13629,
#13630,#13631,#13632,#13633,#13634,#13635,#13636,#13637,#13638,#13639,#13640,
#13641,#13642,#13643,#13644,#13645,#13646,#13647,#13648,#13649,#13650,#13651,
#13652,#13653,#13654,#13655,#13656,#13657,#13658,#13659,#13660,#13661,#13662,
#13663,#13664,#13665,#13666,#13667,#13668,#13669,#13670,#13671,#13672,#13673,
#13674,#13675,#13676,#13677,#13678,#13679,#13680,#13681,#13682,#13683,#13684,
#13685,#13686,#13687,#13688,#13689,#13690,#13691,#13692,#13693,#13694,#13695,
#13696,#13697,#13698,#13699,#13700,#13701,#13702,#13703,#13704,#13705,#13706,
#13707,#13708,#13709,#13710,#13711,#13712,#13713,#13714,#13715,#13716,#13717,
#13718,#13719,#13720,#13721,#13722,#13723,#13724,#13725,#13726,#13727,#13728,
#13729,#13730,#13731,#13732),.UNSPECIFIED.,.F.,.F.,(4,3,3,3,3,3,3,3,3,3,
3,3,3,3,3,3,3,3,3,3,3,3,3,3,3,3,3,3,3,3,3,3,3,3,3,3,3,3,3,3,3,3,3,4),(59.6902604184509,
59.7891705930349,59.8879576408718,59.9866781469733,60.0853650263375,60.1840511466361,
60.2828331759564,60.3816669914442,60.4806673091668,60.5400185568728,60.6405221893055,
60.7408804445777,60.8411217588202,60.941299106129,61.0414437400829,61.1415868732625,
61.2418299508799,61.3421210342123,61.442595067247,61.5384876529759,61.6389912978506,
61.739349565851,61.8395908931883,61.9397682538086,62.0399129012705,62.1400560481343,
62.2402991396139,62.3405902369283,62.4410642839787,62.5369567490791,62.637460269328,
62.7378184124023,62.8380596149486,62.938236850914,63.0383813740269,63.1385243970175,
63.2387673662416,63.3390583419822,63.4395322700663,63.5354258451822,63.6359001279754,
63.7362475749873,63.8364882533271,63.9272632692833),.UNSPECIFIED.);
#140=B_SPLINE_CURVE_WITH_KNOTS('',3,(#13738,#13739,#13740,#13741,#13742,
#13743,#13744,#13745,#13746,#13747,#13748,#13749,#13750,#13751,#13752,#13753,
#13754,#13755,#13756,#13757,#13758,#13759,#13760,#13761,#13762,#13763,#13764,
#13765,#13766,#13767,#13768,#13769,#13770,#13771,#13772,#13773,#13774,#13775,
#13776,#13777,#13778,#13779,#13780,#13781,#13782,#13783,#13784,#13785,#13786,
#13787,#13788,#13789,#13790,#13791,#13792,#13793,#13794,#13795,#13796,#13797,
#13798,#13799,#13800,#13801,#13802,#13803,#13804,#13805,#13806,#13807,#13808,
#13809,#13810,#13811,#13812,#13813,#13814,#13815,#13816,#13817,#13818,#13819,
#13820,#13821,#13822,#13823,#13824,#13825,#13826,#13827,#13828,#13829,#13830,
#13831,#13832,#13833,#13834,#13835,#13836,#13837,#13838,#13839,#13840,#13841,
#13842,#13843,#13844,#13845,#13846,#13847,#13848,#13849,#13850,#13851,#13852,
#13853,#13854,#13855,#13856,#13857,#13858,#13859,#13860,#13861,#13862,#13863,
#13864),.UNSPECIFIED.,.F.,.F.,(4,3,3,3,3,3,3,3,3,3,3,3,3,3,3,3,3,3,3,3,
3,3,3,3,3,3,3,3,3,3,3,3,3,3,3,3,3,3,3,3,3,3,4),(65.9734457256259,66.1045621138705,
66.2186851263839,66.319204460379,66.4195783751114,66.5198352129705,66.6200279947471,
66.7201879536106,66.8203462816385,66.9206042438911,67.020910067048,67.1213984191851,
67.217154222487,67.3176605765936,67.4180217399506,67.5182662262134,67.6184469040974,
67.7185950211813,67.8187417841957,67.9189886942884,68.0192837268467,68.1197618581208,
68.2156233185902,68.3160501801306,68.4163314235567,68.5164957231465,68.6165960861905,
68.7166638700256,68.8167303910506,68.9168977673635,69.0171135203952,69.1175137527569,
69.2140924146934,69.3147586491318,69.4152792017634,69.5156814856034,69.6160189639454,
69.7163226726744,69.8166236057553,69.917020695783,70.0174643709433,70.1180849250332,
70.2101735890481),.UNSPECIFIED.);
#141=B_SPLINE_CURVE_WITH_KNOTS('',3,(#13865,#13866,#13867,#13868,#13869,
#13870,#13871,#13872,#13873,#13874,#13875,#13876,#13877,#13878,#13879,#13880,
#13881,#13882,#13883,#13884,#13885,#13886,#13887,#13888,#13889,#13890,#13891,
#13892,#13893,#13894,#13895,#13896,#13897,#13898,#13899,#13900,#13901,#13902,
#13903,#13904,#13905,#13906,#13907,#13908,#13909,#13910,#13911,#13912,#13913,
#13914,#13915,#13916,#13917,#13918,#13919,#13920,#13921,#13922,#13923,#13924,
#13925,#13926,#13927,#13928),.UNSPECIFIED.,.F.,.F.,(4,3,3,3,3,3,3,3,3,3,
3,3,3,3,3,3,3,3,3,3,3,4),(63.9264178079843,64.0267110513925,64.1271867727341,
64.2217469341776,64.3222514687351,64.4226106459022,64.5228529071813,64.6230312163507,
64.7231768255406,64.8233209458962,64.9235650222929,65.0238571123659,65.1243321534556,
65.2202160302807,65.3194873449581,65.4186277683698,65.5176701627707,65.6166472647161,
65.7156217782399,65.8145923419986,65.9136431342839,65.9734457253857),
 .UNSPECIFIED.);
#142=B_SPLINE_CURVE_WITH_KNOTS('',3,(#13930,#13931,#13932,#13933,#13934,
#13935,#13936,#13937,#13938,#13939,#13940,#13941,#13942,#13943,#13944,#13945,
#13946,#13947,#13948,#13949,#13950,#13951,#13952,#13953,#13954,#13955,#13956,
#13957,#13958,#13959,#13960,#13961,#13962,#13963,#13964,#13965,#13966,#13967,
#13968,#13969,#13970,#13971,#13972,#13973,#13974,#13975,#13976,#13977,#13978,
#13979,#13980,#13981,#13982,#13983,#13984,#13985,#13986,#13987,#13988,#13989,
#13990),.UNSPECIFIED.,.F.,.F.,(4,3,3,3,3,3,3,3,3,3,3,3,3,3,3,3,3,3,3,3,
4),(63.9272632692833,64.027409768621,64.1275518239694,64.2291376032984,
64.3294238753586,64.431659408322,64.5338949412854,64.6343987230996,64.7347571298614,
64.8349985980259,64.9351761006638,65.0353208911287,65.1354641817773,65.2357074172405,
65.3359986588827,65.4364728491071,65.5323640373885,65.6426344593317,65.7510908781998,
65.8622683016806,65.9734457251614),.UNSPECIFIED.);
#143=B_SPLINE_CURVE_WITH_KNOTS('',3,(#13991,#13992,#13993,#13994,#13995,
#13996,#13997,#13998,#13999,#14000,#14001,#14002,#14003,#14004,#14005,#14006,
#14007,#14008,#14009,#14010,#14011,#14012,#14013,#14014,#14015,#14016,#14017,
#14018,#14019,#14020,#14021,#14022,#14023,#14024,#14025,#14026,#14027,#14028,
#14029,#14030,#14031,#14032,#14033,#14034,#14035,#14036,#14037,#14038,#14039,
#14040,#14041,#14042,#14043,#14044,#14045,#14046,#14047,#14048,#14049,#14050,
#14051,#14052,#14053,#14054,#14055,#14056,#14057,#14058,#14059,#14060,#14061,
#14062,#14063,#14064,#14065,#14066,#14067,#14068,#14069,#14070,#14071,#14072,
#14073,#14074,#14075,#14076,#14077,#14078,#14079,#14080,#14081,#14082,#14083,
#14084,#14085,#14086,#14087,#14088,#14089,#14090,#14091,#14092,#14093,#14094,
#14095,#14096,#14097,#14098,#14099,#14100,#14101,#14102,#14103,#14104,#14105,
#14106,#14107,#14108,#14109,#14110,#14111,#14112,#14113,#14114),
 .UNSPECIFIED.,.F.,.F.,(4,2,2,2,2,2,2,2,2,2,2,2,2,2,2,2,2,2,2,2,2,2,2,2,
2,2,2,2,2,2,2,2,2,2,2,2,2,2,2,2,2,2,2,2,2,2,2,2,2,2,2,2,2,2,2,2,2,2,2,2,
2,4),(1.00824602608924,1.01205513967596,1.03667147698884,1.04617077086747,
1.05289638644987,1.0600033393827,1.07118494539582,1.08461203483999,1.11432236538005,
1.1582731364538,1.16588397620221,1.17012602038236,1.17398428622679,1.17972406798352,
1.19726737246127,1.23322199901602,1.27199065073597,1.28242399916394,1.28938061641006,
1.29627970850104,1.30640730244607,1.34074553538651,1.38569495102374,1.3998852090954,
1.40537117310134,1.40918795999741,1.41353750104416,1.42167990919704,1.45247726894626,
1.50791683688854,1.51910257343983,1.52620832597893,1.53300661870801,1.54255149865627,
1.56961368256385,1.63149630630471,1.64010845803438,1.64455166958707,1.64834654686455,
1.65366057885852,1.66759412848501,1.69134875213895,1.74485775571996,1.75630106280688,
1.76345772337208,1.77022861621261,1.77960834947042,1.80509733750006,1.85634316578921,
1.87390085041281,1.87979203383812,1.88363963617856,1.88781230588131,1.89509401479404,
1.93179614934836,1.94577129543914,1.96746683854864,1.9878688856724,1.99668867561983,
2.00326526097165,2.00959291509812,2.01574395093934),.UNSPECIFIED.);
#144=B_SPLINE_CURVE_WITH_KNOTS('',3,(#14122,#14123,#14124,#14125,#14126),
 .UNSPECIFIED.,.F.,.F.,(4,1,4),(0.,0.99846909610315,1.11730040836818),
 .UNSPECIFIED.);
#145=B_SPLINE_CURVE_WITH_KNOTS('',3,(#14128,#14129,#14130,#14131,#14132,
#14133,#14134,#14135,#14136,#14137,#14138,#14139,#14140,#14141,#14142,#14143,
#14144,#14145,#14146,#14147,#14148,#14149,#14150,#14151,#14152,#14153,#14154,
#14155,#14156,#14157,#14158,#14159,#14160,#14161,#14162,#14163,#14164,#14165,
#14166,#14167,#14168,#14169,#14170,#14171,#14172,#14173,#14174,#14175,#14176,
#14177,#14178,#14179,#14180,#14181,#14182,#14183,#14184,#14185,#14186,#14187,
#14188,#14189,#14190,#14191,#14192,#14193,#14194,#14195,#14196,#14197,#14198,
#14199,#14200,#14201,#14202,#14203,#14204,#14205,#14206,#14207,#14208,#14209,
#14210,#14211,#14212,#14213,#14214,#14215,#14216,#14217,#14218,#14219,#14220,
#14221,#14222,#14223,#14224,#14225,#14226,#14227,#14228,#14229,#14230,#14231,
#14232,#14233,#14234,#14235,#14236,#14237,#14238,#14239,#14240,#14241,#14242,
#14243,#14244,#14245,#14246,#14247,#14248,#14249,#14250,#14251,#14252,#14253,
#14254,#14255,#14256,#14257,#14258,#14259,#14260,#14261,#14262,#14263,#14264,
#14265,#14266,#14267,#14268,#14269,#14270,#14271,#14272,#14273,#14274,#14275,
#14276,#14277,#14278,#14279,#14280,#14281,#14282,#14283,#14284,#14285,#14286,
#14287,#14288,#14289,#14290,#14291,#14292,#14293,#14294,#14295,#14296,#14297,
#14298,#14299,#14300,#14301,#14302,#14303,#14304,#14305,#14306,#14307,#14308,
#14309,#14310,#14311,#14312,#14313,#14314,#14315,#14316,#14317,#14318,#14319,
#14320,#14321,#14322,#14323,#14324,#14325,#14326,#14327,#14328,#14329,#14330,
#14331,#14332,#14333,#14334,#14335),.UNSPECIFIED.,.F.,.F.,(4,3,3,3,3,3,
3,3,3,3,3,3,3,3,3,3,3,3,3,3,3,3,3,3,3,3,3,3,3,3,3,3,3,3,3,3,3,3,3,3,3,3,
3,3,3,3,3,3,3,3,3,3,3,3,3,3,3,3,3,3,3,3,3,3,3,3,3,3,3,4),(1.11730040836818,
1.21065985735401,1.30390194475301,1.39705744064107,1.4901678784628,1.58326153126441,
1.67636664830859,1.76956843076783,1.86282531823738,1.95623097050921,1.9969381922063,
2.09215365785623,2.18723546969277,2.28221324248444,2.37711927198641,2.47198876703138,
2.56684832311444,2.66172451959558,2.75670224342694,2.85173672319016,2.94692297821923,
2.99540728830945,3.09078086916065,3.18602566035351,3.28117100808536,3.37625073396202,
3.47129765490557,3.56633814252046,3.66139855523426,3.75656435213686,3.85178937367802,
3.94716814873181,3.9938763844126,4.08904010196092,4.18407158401662,4.27900049979211,
4.37386006033638,4.4686845838142,4.56350071865504,4.65833509850859,4.75327369195789,
4.84827050870551,4.94342174995638,4.99234548051575,5.08758258885795,5.18268824482578,
5.27769200953076,5.37262710940974,5.46752757297348,5.56241995503605,5.6573307958684,
5.75234570846594,5.8474188782428,5.94264577720095,5.99081457661891,6.08606120666011,
6.18117674991679,6.27619075171994,6.37113656826171,6.46604804239538,6.56095171605648,
6.65587411687473,6.75090092855928,6.8459862080092,6.94122542766207,6.98928367272206,
7.09421646824028,7.19886064554355,7.30299800135061,7.4004857153595),
 .UNSPECIFIED.);
#146=B_SPLINE_CURVE_WITH_KNOTS('',3,(#14337,#14338,#14339,#14340,#14341,
#14342,#14343,#14344,#14345,#14346,#14347,#14348,#14349,#14350,#14351,#14352,
#14353,#14354,#14355,#14356,#14357,#14358,#14359,#14360,#14361,#14362,#14363,
#14364,#14365,#14366,#14367,#14368,#14369,#14370,#14371,#14372,#14373,#14374,
#14375,#14376,#14377,#14378,#14379,#14380,#14381,#14382,#14383,#14384,#14385,
#14386,#14387,#14388,#14389,#14390,#14391,#14392,#14393,#14394,#14395,#14396,
#14397,#14398,#14399,#14400,#14401,#14402,#14403,#14404,#14405,#14406,#14407,
#14408,#14409,#14410,#14411,#14412,#14413,#14414,#14415,#14416,#14417,#14418,
#14419,#14420,#14421,#14422,#14423,#14424,#14425,#14426,#14427,#14428,#14429,
#14430,#14431,#14432,#14433,#14434,#14435,#14436,#14437,#14438,#14439,#14440,
#14441,#14442,#14443,#14444,#14445,#14446,#14447,#14448,#14449,#14450,#14451,
#14452,#14453,#14454,#14455,#14456,#14457,#14458,#14459,#14460,#14461,#14462,
#14463,#14464,#14465,#14466,#14467,#14468,#14469,#14470,#14471,#14472,#14473,
#14474,#14475,#14476,#14477,#14478,#14479,#14480,#14481,#14482,#14483,#14484,
#14485,#14486,#14487,#14488,#14489,#14490,#14491,#14492,#14493,#14494,#14495,
#14496,#14497,#14498,#14499,#14500,#14501,#14502,#14503,#14504,#14505,#14506,
#14507,#14508,#14509,#14510,#14511,#14512,#14513,#14514,#14515,#14516,#14517,
#14518,#14519,#14520,#14521,#14522,#14523,#14524,#14525,#14526,#14527,#14528,
#14529,#14530,#14531,#14532,#14533,#14534,#14535,#14536,#14537,#14538,#14539,
#14540,#14541,#14542,#14543,#14544),.UNSPECIFIED.,.F.,.F.,(4,3,3,3,3,3,
3,3,3,3,3,3,3,3,3,3,3,3,3,3,3,3,3,3,3,3,3,3,3,3,3,3,3,3,3,3,3,3,3,3,3,3,
3,3,3,3,3,3,3,3,3,3,3,3,3,3,3,3,3,3,3,3,3,3,3,3,3,3,3,4),(7.40048571554785,
7.49694862342332,7.59345175867044,7.69202701120913,7.78874679069572,7.88824977976047,
7.98775276882521,8.08298690953471,8.17808970347387,8.27309071538798,8.36802323803583,
8.46292123452626,8.55781126324666,8.65271986814037,8.74773273812048,8.84280397222948,
8.93802912200363,8.98622186492836,9.08145627199536,9.17655935994665,9.27156069298133,
9.36649357595562,9.46139195700295,9.55628239411369,9.6511914308544,9.74620476588071,
9.84127648461411,9.936502144916,9.98469096103151,10.0799232949096,10.1750242723557,
10.2700234607491,10.3649541572306,10.4598503266232,10.5547385296284,10.6496453125056,
10.7446563773396,10.8397258132155,10.934949193209,10.9831600571347,11.0783933910534,
11.1734953814528,11.2684955942089,11.3634273277133,11.4583245415938,11.5532137952553,
11.6481216336654,11.7431337549892,11.8382042494707,11.9334286810046,11.9816291532378,
12.0768624375003,12.1719643799482,12.2669645465182,12.3618962366793,12.4567934090009,
12.5516826229467,12.6465904235459,12.7416025102032,12.8366729717551,12.9318973734026,
12.980098249341,13.0746871478763,13.1691531641134,13.2635237606834,13.3578263005673,
13.4521042028511,13.54636740019,13.6406740486691,13.6836710227273),
 .UNSPECIFIED.);
#147=B_SPLINE_CURVE_WITH_KNOTS('',3,(#14546,#14547,#14548,#14549,#14550,
#14551,#14552,#14553,#14554,#14555,#14556,#14557,#14558,#14559,#14560,#14561,
#14562,#14563,#14564,#14565,#14566,#14567,#14568,#14569,#14570,#14571,#14572,
#14573,#14574,#14575,#14576,#14577,#14578,#14579,#14580,#14581,#14582,#14583,
#14584,#14585,#14586,#14587,#14588,#14589,#14590,#14591,#14592,#14593,#14594,
#14595,#14596,#14597,#14598,#14599,#14600,#14601,#14602,#14603,#14604,#14605,
#14606,#14607,#14608,#14609,#14610,#14611,#14612,#14613,#14614,#14615,#14616,
#14617,#14618,#14619,#14620,#14621,#14622,#14623,#14624,#14625,#14626,#14627,
#14628,#14629,#14630,#14631,#14632,#14633,#14634,#14635,#14636,#14637,#14638,
#14639,#14640,#14641,#14642,#14643,#14644,#14645,#14646,#14647,#14648,#14649,
#14650,#14651,#14652,#14653,#14654,#14655,#14656,#14657,#14658,#14659,#14660,
#14661,#14662,#14663,#14664,#14665,#14666,#14667,#14668,#14669,#14670,#14671,
#14672,#14673,#14674,#14675,#14676,#14677,#14678,#14679,#14680,#14681,#14682,
#14683,#14684,#14685,#14686,#14687,#14688,#14689,#14690,#14691,#14692,#14693,
#14694,#14695,#14696,#14697,#14698,#14699,#14700,#14701,#14702,#14703,#14704,
#14705,#14706,#14707,#14708,#14709,#14710,#14711,#14712,#14713,#14714,#14715,
#14716,#14717,#14718,#14719,#14720,#14721,#14722,#14723,#14724,#14725,#14726,
#14727,#14728,#14729,#14730,#14731,#14732,#14733,#14734,#14735,#14736,#14737,
#14738,#14739,#14740,#14741,#14742,#14743,#14744,#14745,#14746,#14747,#14748,
#14749,#14750,#14751,#14752,#14753),.UNSPECIFIED.,.F.,.F.,(4,3,3,3,3,3,
3,3,3,3,3,3,3,3,3,3,3,3,3,3,3,3,3,3,3,3,3,3,3,3,3,3,3,3,3,3,3,3,3,3,3,3,
3,3,3,3,3,3,3,3,3,3,3,3,3,3,3,3,3,3,3,3,3,3,3,3,3,3,3,4),(13.6836710230158,
13.7985703413321,13.9151166307046,13.9785673454441,14.0738005443357,14.1689023992021,
14.2639024761147,14.3588340738977,14.4537311521857,14.5486202705559,14.6435279741488,
14.7385399622103,14.8336103241159,14.9288346254482,14.9770364415473,15.0722696271906,
15.1673714688582,15.26237153264,15.3573031174507,15.4522001828701,15.5470892884921,
15.6419969794739,15.7370089552118,15.8320793049388,15.9273035944392,15.9755055376504,
16.0707387051867,16.1658405283805,16.26084057335,16.3557721389227,16.4506691848468,
16.5455582707402,16.6404659417835,16.7354778973849,16.8305482268328,16.9257724960296,
16.9739746337536,17.0692078134899,17.1643096490601,17.2593097065639,17.3542412848531,
17.4491383436021,17.5440274424128,17.6389351264502,17.7339470950829,17.8290174376026,
17.9242417198066,17.9724437298567,18.0676769073885,18.1627787407457,18.2577787960312,
18.3527103721036,18.4476074286378,18.5424965252383,18.637404207073,18.732416173528,
18.8274865138812,18.9227107939571,18.9709128259599,19.066102612376,19.1611610822308,
19.2561178627604,19.3510063526438,19.4458605160811,19.5407069670992,19.6355723055026,
19.7305419746598,19.8255703930562,19.9207520511273,19.966856329907),
 .UNSPECIFIED.);
#148=B_SPLINE_CURVE_WITH_KNOTS('',3,(#14755,#14756,#14757,#14758,#14759,
#14760,#14761,#14762,#14763,#14764,#14765,#14766,#14767,#14768,#14769,#14770,
#14771,#14772,#14773,#14774,#14775,#14776,#14777,#14778,#14779,#14780,#14781,
#14782,#14783,#14784,#14785,#14786,#14787,#14788,#14789,#14790,#14791,#14792,
#14793,#14794,#14795,#14796,#14797,#14798,#14799,#14800,#14801,#14802,#14803,
#14804,#14805,#14806,#14807,#14808,#14809,#14810,#14811,#14812,#14813,#14814,
#14815,#14816,#14817,#14818,#14819,#14820,#14821,#14822,#14823,#14824,#14825,
#14826,#14827,#14828,#14829,#14830,#14831,#14832,#14833,#14834,#14835,#14836,
#14837,#14838,#14839,#14840,#14841,#14842,#14843,#14844,#14845,#14846,#14847,
#14848,#14849,#14850,#14851,#14852,#14853,#14854,#14855,#14856,#14857,#14858,
#14859,#14860,#14861,#14862,#14863,#14864,#14865,#14866,#14867,#14868,#14869,
#14870,#14871,#14872,#14873,#14874,#14875,#14876,#14877,#14878,#14879,#14880,
#14881,#14882,#14883,#14884,#14885,#14886,#14887,#14888,#14889,#14890,#14891,
#14892,#14893,#14894,#14895,#14896,#14897,#14898,#14899,#14900,#14901,#14902,
#14903,#14904,#14905,#14906,#14907,#14908,#14909,#14910,#14911,#14912,#14913,
#14914,#14915,#14916,#14917,#14918,#14919,#14920,#14921,#14922,#14923,#14924,
#14925,#14926,#14927,#14928,#14929,#14930,#14931,#14932,#14933,#14934,#14935,
#14936,#14937,#14938,#14939,#14940,#14941,#14942,#14943,#14944,#14945,#14946,
#14947,#14948,#14949,#14950,#14951,#14952,#14953,#14954,#14955,#14956,#14957,
#14958,#14959,#14960,#14961,#14962,#14963,#14964,#14965),.UNSPECIFIED.,
 .F.,.F.,(4,3,3,3,3,3,3,3,3,3,3,3,3,3,3,3,3,3,3,3,3,3,3,3,3,3,3,3,3,3,3,
3,3,3,3,3,3,3,3,3,3,3,3,3,3,3,3,3,3,3,3,3,3,3,3,3,3,3,3,3,3,3,3,3,3,3,3,
3,3,3,4),(19.9668563310701,19.969381922063,20.0646150993086,20.1597169323645,
20.2547169873338,20.3496485630696,20.4445456192546,20.5394347154935,20.6343423969547,
20.7293543630204,20.8244247029744,20.9196489826402,20.9678510181662,21.0630841950999,
21.1581860278414,21.2531860824947,21.348117657913,21.4430147137796,21.5379038096999,
21.6328114908426,21.7278234565917,21.82289379623,21.918118075584,21.9663201142693,
22.0615532910726,22.1566551236806,22.2516551781973,22.3465867534752,22.4414838091989,
22.5363729049742,22.6312805859698,22.7262925515696,22.8213628910571,22.9165871702596,
22.9647892103725,23.0600223873118,23.1551242200579,23.2501242747148,23.345055850135,
23.4399529060026,23.5348420019228,23.6297496830645,23.724761648811,23.8198319884458,
23.9150562677951,23.9632583064756,24.0584914833744,24.1535933160796,24.2485933706953,
24.343524946074,24.4384220018998,24.5333110977782,24.6282187788779,24.7232307445827,
24.8183010841758,24.9135253634839,24.9617274025788,25.0569605794681,25.1520624121635,
25.247062466769,25.3419940421372,25.4368910979524,25.53178019382,25.6266878749087,
25.7216998406021,25.8167701801838,25.9119944594803,25.9601964986819,26.0776664416472,
26.1934396858132,26.2500416368193),.UNSPECIFIED.);
#149=B_SPLINE_CURVE_WITH_KNOTS('',3,(#14967,#14968,#14969,#14970,#14971,
#14972,#14973,#14974,#14975,#14976,#14977,#14978,#14979,#14980,#14981,#14982,
#14983,#14984,#14985,#14986,#14987,#14988,#14989,#14990,#14991,#14992,#14993,
#14994,#14995,#14996,#14997,#14998,#14999,#15000,#15001,#15002,#15003,#15004,
#15005,#15006,#15007,#15008,#15009,#15010,#15011,#15012,#15013,#15014,#15015,
#15016,#15017,#15018,#15019,#15020,#15021,#15022,#15023,#15024,#15025,#15026,
#15027,#15028,#15029,#15030,#15031,#15032,#15033,#15034,#15035,#15036,#15037,
#15038,#15039,#15040,#15041,#15042,#15043,#15044,#15045,#15046,#15047,#15048,
#15049,#15050,#15051,#15052,#15053,#15054,#15055,#15056,#15057,#15058,#15059,
#15060,#15061,#15062,#15063,#15064,#15065,#15066,#15067,#15068,#15069,#15070,
#15071,#15072,#15073,#15074,#15075,#15076,#15077,#15078,#15079,#15080,#15081,
#15082,#15083,#15084,#15085,#15086,#15087,#15088,#15089,#15090,#15091,#15092,
#15093,#15094,#15095,#15096,#15097,#15098,#15099,#15100,#15101,#15102,#15103,
#15104,#15105,#15106,#15107,#15108,#15109,#15110,#15111,#15112,#15113,#15114,
#15115,#15116,#15117,#15118,#15119,#15120,#15121,#15122,#15123,#15124,#15125,
#15126,#15127,#15128,#15129,#15130,#15131,#15132,#15133,#15134,#15135,#15136,
#15137,#15138,#15139,#15140,#15141,#15142,#15143,#15144,#15145,#15146,#15147,
#15148,#15149,#15150,#15151,#15152,#15153,#15154,#15155,#15156,#15157,#15158,
#15159,#15160,#15161,#15162,#15163,#15164,#15165,#15166,#15167,#15168,#15169,
#15170,#15171,#15172,#15173,#15174),.UNSPECIFIED.,.F.,.F.,(4,3,3,3,3,3,
3,3,3,3,3,3,3,3,3,3,3,3,3,3,3,3,3,3,3,3,3,3,3,3,3,3,3,3,3,3,3,3,3,3,3,3,
3,3,3,3,3,3,3,3,3,3,3,3,3,3,3,3,3,3,3,3,3,3,3,3,3,3,3,4),(26.2500416370864,
26.3442956412353,26.4385114134094,26.5327162678039,26.626937501813,26.7212619406864,
26.815644110387,26.910181456667,26.9586655947851,27.0538987716832,27.1490006043877,
27.2440006590025,27.3389322343801,27.4338292902048,27.528718386082,27.6236260671802,
27.7186380328836,27.8137083724751,27.9089326517814,27.9571346908882,28.0523678677858,
28.1474697004896,28.2424697551041,28.3374013304812,28.4322983863053,28.5271874821818,
28.6220951632799,28.7171071289826,28.8121774685736,28.9074017478793,28.9556037869914,
29.0508369638904,29.1459387965958,29.2409388512117,29.3358704265903,29.4307674824158,
29.5256565782939,29.6205642593929,29.7155762250971,29.8106465646894,29.9058708439967,
29.9540728830945,30.0493060599929,30.1444078926975,30.2394079473122,30.3343395226901,
30.4292365785151,30.5241256743925,30.6190333554911,30.7140453211946,30.8091156607864,
30.9043399400928,30.9525419791977,31.0477751560962,31.142876988801,31.2378770434165,
31.3328086187944,31.4277056746193,31.5225947704971,31.617502451596,31.7125144172995,
31.8075847568911,31.9028090361976,31.9510110753008,32.0481125083967,32.1450646576551,
32.2421052293078,32.3388092131387,32.4360180787024,32.5332269442661),
 .UNSPECIFIED.);
#150=B_SPLINE_CURVE_WITH_KNOTS('',3,(#15176,#15177,#15178,#15179,#15180,
#15181,#15182,#15183,#15184,#15185,#15186,#15187,#15188,#15189,#15190,#15191,
#15192,#15193,#15194,#15195,#15196,#15197,#15198,#15199,#15200,#15201,#15202,
#15203,#15204,#15205,#15206,#15207,#15208,#15209,#15210,#15211,#15212,#15213,
#15214,#15215,#15216,#15217,#15218,#15219,#15220,#15221,#15222,#15223,#15224,
#15225,#15226,#15227,#15228,#15229,#15230,#15231,#15232,#15233,#15234,#15235,
#15236,#15237,#15238,#15239,#15240,#15241,#15242,#15243,#15244,#15245,#15246,
#15247,#15248,#15249,#15250,#15251,#15252,#15253,#15254,#15255,#15256,#15257,
#15258,#15259,#15260,#15261,#15262,#15263,#15264,#15265,#15266,#15267,#15268,
#15269,#15270,#15271,#15272,#15273,#15274,#15275,#15276,#15277,#15278,#15279,
#15280,#15281,#15282,#15283,#15284,#15285,#15286,#15287,#15288,#15289,#15290,
#15291,#15292,#15293,#15294,#15295,#15296,#15297,#15298,#15299,#15300,#15301,
#15302,#15303,#15304,#15305,#15306,#15307,#15308,#15309,#15310,#15311,#15312,
#15313,#15314,#15315,#15316,#15317,#15318,#15319,#15320,#15321,#15322,#15323,
#15324,#15325,#15326,#15327,#15328,#15329,#15330,#15331,#15332,#15333,#15334,
#15335,#15336,#15337,#15338,#15339,#15340,#15341,#15342,#15343,#15344,#15345,
#15346,#15347,#15348,#15349,#15350,#15351,#15352,#15353,#15354,#15355,#15356,
#15357,#15358,#15359,#15360,#15361,#15362,#15363,#15364,#15365,#15366,#15367,
#15368,#15369,#15370,#15371,#15372,#15373,#15374,#15375,#15376,#15377,#15378,
#15379,#15380,#15381,#15382,#15383),.UNSPECIFIED.,.F.,.F.,(4,3,3,3,3,3,
3,3,3,3,3,3,3,3,3,3,3,3,3,3,3,3,3,3,3,3,3,3,3,3,3,3,3,3,3,3,3,3,3,3,3,3,
3,3,3,3,3,3,3,3,3,3,3,3,3,3,3,3,3,3,3,3,3,3,3,3,3,3,3,4),(32.5332269444471,
32.6372902511863,32.7414250445488,32.8460277844409,32.949480171404,33.0447133483024,
33.139815181007,33.2348152356221,33.3297468109999,33.4246438668248,33.5195329627023,
33.6144406438008,33.7094526095044,33.804522949096,33.8997472284026,33.9479492675071,
34.0431824444056,34.1382842771103,34.2332843317255,34.3282159071034,34.4231129629284,
34.5180020588059,34.6129097399045,34.7079217056081,34.8029920451999,34.8982163245065,
34.9464183636103,35.0416515405094,35.1367533732147,35.2317534278304,35.326685003209,
35.4215820590346,35.5164711549127,35.611378836012,35.7063908017162,35.8014611413086,
35.8966854206158,35.9448874597135,36.040120636611,36.1352224693148,36.2302225239289,
36.325154099306,36.42005115513,36.5149402510066,36.6098479321044,36.704859897807,
36.7999302373979,36.8951545167037,36.9433565558166,37.0385897327149,37.1336915654195,
37.2286916200344,37.3236231954121,37.4185202512368,37.5134093471141,37.6083170282125,
37.7033289939159,37.7983993335075,37.8936236128138,37.9418256519198,38.0357356109504,
38.133320190983,38.2269898496088,38.320602829707,38.4141870665519,38.5077704591112,
38.6014277414157,38.6951291379142,38.788953707224,38.8164122512114),
 .UNSPECIFIED.);
#151=B_SPLINE_CURVE_WITH_KNOTS('',3,(#15385,#15386,#15387,#15388,#15389,
#15390,#15391,#15392,#15393,#15394,#15395,#15396,#15397,#15398,#15399,#15400,
#15401,#15402,#15403,#15404,#15405,#15406,#15407,#15408,#15409,#15410,#15411,
#15412,#15413,#15414,#15415,#15416,#15417,#15418,#15419,#15420,#15421,#15422,
#15423,#15424,#15425,#15426,#15427,#15428,#15429,#15430,#15431,#15432,#15433,
#15434,#15435,#15436,#15437,#15438,#15439,#15440,#15441,#15442,#15443,#15444,
#15445,#15446,#15447,#15448,#15449,#15450,#15451,#15452,#15453,#15454,#15455,
#15456,#15457,#15458,#15459,#15460,#15461,#15462,#15463,#15464,#15465,#15466,
#15467,#15468,#15469,#15470,#15471,#15472,#15473,#15474,#15475,#15476,#15477,
#15478,#15479,#15480,#15481,#15482,#15483,#15484,#15485,#15486,#15487,#15488,
#15489,#15490,#15491,#15492,#15493,#15494,#15495,#15496,#15497,#15498,#15499,
#15500,#15501,#15502,#15503,#15504,#15505,#15506,#15507,#15508,#15509,#15510,
#15511,#15512,#15513,#15514,#15515,#15516,#15517,#15518,#15519,#15520,#15521,
#15522,#15523,#15524,#15525,#15526,#15527,#15528,#15529,#15530,#15531,#15532,
#15533,#15534,#15535,#15536,#15537,#15538,#15539,#15540,#15541,#15542,#15543,
#15544,#15545,#15546,#15547,#15548,#15549,#15550,#15551,#15552,#15553,#15554,
#15555,#15556,#15557,#15558,#15559,#15560,#15561,#15562,#15563,#15564,#15565,
#15566,#15567,#15568,#15569,#15570,#15571,#15572,#15573,#15574,#15575,#15576,
#15577,#15578,#15579,#15580,#15581,#15582,#15583,#15584,#15585,#15586,#15587,
#15588,#15589,#15590,#15591,#15592),.UNSPECIFIED.,.F.,.F.,(4,3,3,3,3,3,
3,3,3,3,3,3,3,3,3,3,3,3,3,3,3,3,3,3,3,3,3,3,3,3,3,3,3,3,3,3,3,3,3,3,3,3,
3,3,3,3,3,3,3,3,3,3,3,3,3,3,3,3,3,3,3,3,3,3,3,3,3,3,3,4),(38.8164122514458,
38.9402947480229,39.0355279249114,39.1306297576062,39.2256298122114,39.3205613875795,
39.4154584433947,39.5103475392625,39.6052552203517,39.7002671860458,39.7953375256283,
39.8905618049258,39.9387638441261,40.0339970210259,40.1290988537319,40.2240989083482,
40.319030483727,40.4139275395529,40.5088166354311,40.6037243165304,40.6987362822345,
40.7938066218268,40.8890309011337,40.9372329402292,41.0324661171702,41.1275679499177,
41.2225680045755,41.3174995799963,41.412396635864,41.5072857317841,41.6021934129253,
41.697205378671,41.7922757183046,41.8874999976523,41.9357020363324,42.0309352131271,
42.1260370457283,42.22103710024,42.3159686755154,42.4108657312383,42.5057548270144,
42.6006625080123,42.6956744736171,42.7907448131109,42.8859690923218,42.9341711324355,
43.0294043093814,43.1245061421326,43.2195061967932,43.314437772215,43.4093348280827,
43.5042239240018,43.5991316051411,43.6941435708833,43.7892139105126,43.8844381898547,
43.9326402285387,44.0278734057947,44.1229752388588,44.2179752938344,44.3129068695732,
44.407803925759,44.5026930219969,44.5976007034551,44.6926126695148,44.7876830094613,
44.8829072891169,44.9311093246418,45.0810523173759,45.0995975586252),
 .UNSPECIFIED.);
#152=B_SPLINE_CURVE_WITH_KNOTS('',3,(#15594,#15595,#15596,#15597,#15598,
#15599,#15600,#15601,#15602,#15603,#15604,#15605,#15606,#15607,#15608,#15609,
#15610,#15611,#15612,#15613,#15614,#15615,#15616,#15617,#15618,#15619,#15620,
#15621,#15622,#15623,#15624,#15625,#15626,#15627,#15628,#15629,#15630,#15631,
#15632,#15633,#15634,#15635,#15636,#15637,#15638,#15639,#15640,#15641,#15642,
#15643,#15644,#15645,#15646,#15647,#15648,#15649,#15650,#15651,#15652,#15653,
#15654,#15655,#15656,#15657,#15658,#15659,#15660,#15661,#15662,#15663,#15664,
#15665,#15666,#15667,#15668,#15669,#15670,#15671,#15672,#15673,#15674,#15675,
#15676,#15677,#15678,#15679,#15680,#15681,#15682,#15683,#15684,#15685,#15686,
#15687,#15688,#15689,#15690,#15691,#15692,#15693,#15694,#15695,#15696,#15697,
#15698,#15699,#15700,#15701,#15702,#15703,#15704,#15705,#15706,#15707,#15708,
#15709,#15710,#15711,#15712,#15713,#15714,#15715,#15716,#15717,#15718,#15719,
#15720,#15721,#15722,#15723,#15724,#15725,#15726,#15727,#15728,#15729,#15730,
#15731,#15732,#15733,#15734,#15735,#15736,#15737,#15738,#15739,#15740,#15741,
#15742,#15743,#15744,#15745,#15746,#15747,#15748,#15749,#15750,#15751,#15752,
#15753,#15754,#15755,#15756,#15757,#15758,#15759,#15760,#15761,#15762,#15763,
#15764,#15765,#15766,#15767,#15768,#15769,#15770,#15771,#15772,#15773,#15774,
#15775,#15776,#15777,#15778,#15779,#15780,#15781,#15782,#15783,#15784,#15785,
#15786,#15787,#15788,#15789,#15790,#15791,#15792,#15793,#15794,#15795,#15796,
#15797,#15798,#15799,#15800,#15801),.UNSPECIFIED.,.F.,.F.,(4,3,3,3,3,3,
3,3,3,3,3,3,3,3,3,3,3,3,3,3,3,3,3,3,3,3,3,3,3,3,3,3,3,3,3,3,3,3,3,3,3,3,
3,3,3,3,3,3,3,3,3,3,3,3,3,3,3,3,3,3,3,3,3,3,3,3,3,3,3,4),(45.0995975587957,
45.1932779352248,45.2868546323476,45.3803749446052,45.473866884399,45.5673584285438,
45.6609386622286,45.7545628987289,45.848346419118,45.929578420745,46.0248115984109,
46.1199134318747,46.2149134872393,46.3098450633499,46.4047421198968,46.4996312164845,
46.5945388982812,46.68955086466,46.7846212049148,46.8798454848594,46.9280475168481,
47.0232806966308,47.1183825322378,47.213382589769,47.3083141680714,47.4032112268248,
47.4981003256312,47.5930080096552,47.6880199782615,47.7830903207475,47.8783146029061,
47.9265166129513,48.0217497797786,48.1168516024089,48.2118516469599,48.3067832123307,
48.4016802581877,48.4965693441479,48.5914770153927,48.6864889713977,48.7815593013646,
48.8767835712549,48.9249857090544,49.0202188961172,49.1153207389126,49.2103208035327,
49.3052523887474,49.4001494543016,49.4950385597896,49.5899462503684,49.6849582252982,
49.7800285739857,49.8752528620976,49.9234548051576,50.0186880039757,50.1137898587833,
50.2087899356529,50.3037215334149,50.3986186116959,50.4935077300731,50.588415433687,
50.6834274217903,50.7784977837497,50.8737220851538,50.9219239012607,51.0239506924649,
51.1256428471772,51.2271277096782,51.3283182871639,51.3827828656131),
 .UNSPECIFIED.);
#153=B_SPLINE_CURVE_WITH_KNOTS('',3,(#15803,#15804,#15805,#15806,#15807,
#15808,#15809,#15810,#15811,#15812,#15813,#15814,#15815,#15816,#15817,#15818,
#15819,#15820,#15821,#15822,#15823,#15824,#15825,#15826,#15827,#15828,#15829,
#15830,#15831,#15832,#15833,#15834,#15835,#15836,#15837,#15838,#15839,#15840,
#15841,#15842,#15843,#15844,#15845,#15846,#15847,#15848,#15849,#15850,#15851,
#15852,#15853,#15854,#15855,#15856,#15857,#15858,#15859,#15860,#15861,#15862,
#15863,#15864,#15865,#15866,#15867,#15868,#15869,#15870,#15871,#15872,#15873,
#15874,#15875,#15876,#15877,#15878,#15879,#15880,#15881,#15882,#15883,#15884,
#15885,#15886,#15887,#15888,#15889,#15890,#15891,#15892,#15893,#15894,#15895,
#15896,#15897,#15898,#15899,#15900,#15901,#15902,#15903,#15904,#15905,#15906,
#15907,#15908,#15909,#15910,#15911,#15912,#15913,#15914,#15915,#15916,#15917,
#15918,#15919,#15920,#15921,#15922,#15923,#15924,#15925,#15926,#15927,#15928,
#15929,#15930,#15931,#15932,#15933,#15934,#15935,#15936,#15937,#15938,#15939,
#15940,#15941,#15942,#15943,#15944,#15945,#15946,#15947,#15948,#15949,#15950,
#15951,#15952,#15953,#15954,#15955,#15956,#15957,#15958,#15959,#15960,#15961,
#15962,#15963,#15964,#15965,#15966,#15967,#15968,#15969,#15970,#15971,#15972,
#15973,#15974,#15975,#15976,#15977,#15978,#15979,#15980,#15981,#15982,#15983,
#15984,#15985,#15986,#15987,#15988,#15989,#15990,#15991,#15992,#15993,#15994,
#15995,#15996,#15997,#15998,#15999,#16000,#16001,#16002,#16003,#16004,#16005,
#16006,#16007,#16008,#16009,#16010),.UNSPECIFIED.,.F.,.F.,(4,3,3,3,3,3,
3,3,3,3,3,3,3,3,3,3,3,3,3,3,3,3,3,3,3,3,3,3,3,3,3,3,3,3,3,3,3,3,3,3,3,3,
3,3,3,3,3,3,3,3,3,3,3,3,3,3,3,3,3,3,3,3,3,3,3,3,3,3,3,4),(51.3827828658049,
51.4807372785994,51.5787843849556,51.6770268854418,51.7753771076044,51.873937487025,
51.9203929973639,52.0156262962162,52.110728250258,52.2057284254395,52.3006601197524,
52.3955572934587,52.4904465060247,52.5853543024792,52.6803663808299,52.7754368316972,
52.8706612190731,52.918862093467,53.0140954217918,53.109197407746,53.2041976172003,
53.2991293491129,53.3940265624625,53.488915816653,53.583823656652,53.6788357811606,
53.7739062797388,53.8691307167445,53.9173311895702,54.0125634707333,54.107664406289,
54.2026635635679,54.2975942450476,54.3924904094359,54.4873786174258,54.5822854152763,
54.6772965101222,54.7723659846023,54.8675894161599,54.9158002856733,55.0110348389498,
55.1061380430872,55.2011394624195,55.2960723870005,55.3909707819247,55.4858612052065,
55.5807702004123,55.675783452194,55.7708550638512,55.8660805811321,55.9142693817765,
56.0095034236643,56.1046061390741,56.1996070926603,56.2945395871862,56.3894375742971,
56.4843276123638,56.5792362453301,56.674249171574,56.7693204780544,56.8645457244948,
56.9127384778796,57.0068921897677,57.1008392901937,57.1946960848869,57.2884904327465,
57.3828598678059,57.4766387039323,57.5713034384583,57.6659681729844),
 .UNSPECIFIED.);
#154=B_SPLINE_CURVE_WITH_KNOTS('',3,(#16012,#16013,#16014,#16015,#16016,
#16017,#16018,#16019,#16020,#16021,#16022,#16023,#16024,#16025,#16026,#16027,
#16028,#16029,#16030,#16031,#16032,#16033,#16034,#16035,#16036,#16037,#16038,
#16039,#16040,#16041,#16042,#16043,#16044,#16045,#16046,#16047,#16048,#16049,
#16050,#16051,#16052,#16053,#16054,#16055,#16056,#16057,#16058,#16059,#16060,
#16061,#16062,#16063,#16064,#16065,#16066,#16067,#16068,#16069,#16070,#16071,
#16072,#16073,#16074,#16075,#16076,#16077,#16078,#16079,#16080,#16081,#16082,
#16083,#16084,#16085,#16086,#16087,#16088,#16089,#16090,#16091,#16092,#16093,
#16094,#16095,#16096,#16097,#16098,#16099,#16100,#16101,#16102,#16103,#16104,
#16105,#16106,#16107,#16108,#16109,#16110,#16111,#16112,#16113,#16114,#16115,
#16116,#16117,#16118,#16119,#16120,#16121,#16122,#16123,#16124,#16125,#16126,
#16127,#16128,#16129,#16130,#16131,#16132,#16133,#16134,#16135,#16136,#16137,
#16138,#16139,#16140,#16141,#16142,#16143,#16144,#16145,#16146,#16147,#16148,
#16149,#16150,#16151,#16152,#16153,#16154,#16155,#16156,#16157,#16158,#16159,
#16160,#16161,#16162,#16163,#16164,#16165,#16166,#16167,#16168,#16169,#16170,
#16171,#16172,#16173,#16174,#16175,#16176,#16177,#16178,#16179,#16180),
 .UNSPECIFIED.,.F.,.F.,(4,3,3,3,3,3,3,3,3,3,3,3,3,3,3,3,3,3,3,3,3,3,3,3,
3,3,3,3,3,3,3,3,3,3,3,3,3,3,3,3,3,3,3,3,3,3,3,3,3,3,3,3,3,3,3,3,4),(57.6659681732708,
57.7902087726151,57.9112075739828,58.0064556392205,58.1015723229298,58.196587171758,
58.2915333966034,58.3864450068061,58.4813485445348,58.5762705374193,58.671296531744,
58.7663807598672,58.8616185754268,58.9096766700859,59.004912436105,59.1000170253905,
59.1950199978214,59.289954715732,59.3848550519149,59.479747560965,59.5746587831537,
59.6696744600382,59.7647486129024,59.8599768249392,59.9081457661891,60.0033062082597,
60.0983350869559,60.193262068454,60.2881206954997,60.3829449061964,60.4777613484371,
60.5725966558729,60.6675371112889,60.7625363234842,60.8576907662809,60.9066148622922,
61.0020019720403,61.0972575100589,61.1924108347871,61.2874943988881,61.3825425880511,
61.4775817760709,61.5726383213704,61.6677963912266,61.7630114770783,61.8583769974531,
61.9050839583954,61.9992755558128,62.0933384919762,62.1872975266918,62.2811999994194,
62.3750735970995,62.4689459722077,62.5629043553239,62.6569055365934,62.7510620984975,
62.8314472505513),.UNSPECIFIED.);
#155=B_SPLINE_CURVE_WITH_KNOTS('',3,(#16184,#16185,#16186,#16187,#16188,
#16189,#16190,#16191),.UNSPECIFIED.,.F.,.F.,(4,1,1,1,1,4),(-64.9004912467048,
-63.9020221506017,-62.9035530544986,-61.9050839583954,-60.9066148622923,
-60.6416007602447),.UNSPECIFIED.);
#156=B_SPLINE_CURVE_WITH_KNOTS('',3,(#16193,#16194,#16195,#16196,#16197,
#16198,#16199,#16200,#16201,#16202,#16203,#16204,#16205,#16206,#16207,#16208,
#16209,#16210,#16211,#16212,#16213,#16214,#16215,#16216,#16217,#16218,#16219,
#16220,#16221,#16222,#16223,#16224,#16225,#16226,#16227,#16228,#16229,#16230,
#16231,#16232,#16233,#16234,#16235,#16236,#16237,#16238,#16239,#16240,#16241,
#16242,#16243,#16244,#16245,#16246,#16247,#16248,#16249,#16250,#16251,#16252,
#16253,#16254,#16255,#16256,#16257,#16258,#16259,#16260,#16261,#16262,#16263,
#16264,#16265,#16266,#16267,#16268,#16269,#16270,#16271,#16272,#16273,#16274,
#16275,#16276,#16277,#16278,#16279,#16280,#16281,#16282,#16283,#16284,#16285,
#16286,#16287,#16288,#16289,#16290,#16291,#16292,#16293,#16294,#16295,#16296,
#16297,#16298,#16299,#16300,#16301,#16302,#16303,#16304,#16305,#16306,#16307,
#16308,#16309,#16310,#16311,#16312,#16313,#16314,#16315,#16316,#16317,#16318,
#16319,#16320,#16321,#16322,#16323,#16324,#16325,#16326,#16327,#16328,#16329,
#16330,#16331,#16332,#16333,#16334,#16335,#16336,#16337,#16338,#16339,#16340,
#16341,#16342,#16343,#16344,#16345,#16346,#16347,#16348,#16349,#16350,#16351,
#16352,#16353,#16354,#16355,#16356,#16357,#16358,#16359,#16360,#16361,#16362,
#16363,#16364,#16365,#16366,#16367,#16368,#16369,#16370,#16371,#16372,#16373,
#16374,#16375,#16376,#16377,#16378,#16379,#16380,#16381,#16382,#16383,#16384,
#16385,#16386,#16387,#16388,#16389,#16390,#16391,#16392,#16393,#16394,#16395,
#16396,#16397,#16398,#16399,#16400),.UNSPECIFIED.,.F.,.F.,(4,3,3,3,3,3,
3,3,3,3,3,3,3,3,3,3,3,3,3,3,3,3,3,3,3,3,3,3,3,3,3,3,3,3,3,3,3,3,3,3,3,3,
3,3,3,3,3,3,3,3,3,3,3,3,3,3,3,3,3,3,3,3,3,3,3,3,3,3,3,4),(-60.6415981847468,
-60.5476350400387,-60.4537214927512,-60.3598299001311,-60.2659326468451,
-60.1719401382506,-60.0778989118986,-59.9836963724679,-59.9081457661891,
-59.8129086437597,-59.7178029735791,-59.6227991945564,-59.527864080263,
-59.4329636022303,-59.3380712056622,-59.2431603503057,-59.148145423244,
-59.0530722390154,-58.9578453257664,-58.909676670086,-58.8144300356268,
-58.7193144878493,-58.6243004814298,-58.529354660147,-58.4344431811965,
-58.3395395026492,-58.2446170968802,-58.149590280176,-58.0545049956603,
-57.9592657709175,-57.9112075739828,-57.8159821428235,-57.720888162612,
-57.6258960555731,-57.530972535854,-57.4360835997414,-57.341202677585,-57.2463032142147,
-57.1512994829464,-57.0562373995538,-56.9610213295851,-56.9127384778797,
-56.8175043351744,-56.7224015392209,-56.6274005252774,-56.5324680005851,
-56.4375700020421,-56.3426799712632,-56.2477713643077,-56.1527584922739,
-56.0576872561126,-55.9624621043086,-55.9142693817765,-55.8190349740819,
-55.7239318854878,-55.6289305517956,-55.5339976681447,-55.4390992864092,
-55.3442088485995,-55.2492998111501,-55.1542864754041,-55.0592147559437,
-54.9639890949103,-54.9158002856733,-54.8179259631399,-54.720211039569,
-54.6226729319707,-54.525238837996,-54.427905479594,-54.3584128775674),
 .UNSPECIFIED.);
#157=B_SPLINE_CURVE_WITH_KNOTS('',3,(#16402,#16403,#16404,#16405,#16406,
#16407,#16408,#16409,#16410,#16411,#16412,#16413,#16414,#16415,#16416,#16417,
#16418,#16419,#16420,#16421,#16422,#16423,#16424,#16425,#16426,#16427,#16428,
#16429,#16430,#16431,#16432,#16433,#16434,#16435,#16436,#16437,#16438,#16439,
#16440,#16441,#16442,#16443,#16444,#16445,#16446,#16447,#16448,#16449,#16450,
#16451,#16452,#16453,#16454,#16455,#16456,#16457,#16458,#16459,#16460,#16461,
#16462,#16463,#16464,#16465,#16466,#16467,#16468,#16469,#16470,#16471,#16472,
#16473,#16474,#16475,#16476,#16477,#16478,#16479,#16480,#16481,#16482,#16483,
#16484,#16485,#16486,#16487,#16488,#16489,#16490,#16491,#16492,#16493,#16494,
#16495,#16496,#16497,#16498,#16499,#16500,#16501,#16502,#16503,#16504,#16505,
#16506,#16507,#16508,#16509,#16510,#16511,#16512,#16513,#16514,#16515,#16516,
#16517,#16518,#16519,#16520,#16521,#16522,#16523,#16524,#16525,#16526,#16527,
#16528,#16529,#16530,#16531,#16532,#16533,#16534,#16535,#16536,#16537,#16538,
#16539,#16540,#16541,#16542,#16543,#16544,#16545,#16546,#16547,#16548,#16549,
#16550,#16551,#16552,#16553,#16554,#16555,#16556,#16557,#16558,#16559,#16560,
#16561,#16562,#16563,#16564,#16565,#16566,#16567,#16568,#16569,#16570,#16571,
#16572,#16573,#16574,#16575,#16576,#16577,#16578,#16579,#16580,#16581,#16582,
#16583,#16584,#16585,#16586,#16587,#16588,#16589,#16590,#16591,#16592,#16593,
#16594,#16595,#16596,#16597,#16598,#16599,#16600,#16601,#16602,#16603,#16604,
#16605,#16606,#16607,#16608,#16609),.UNSPECIFIED.,.F.,.F.,(4,3,3,3,3,3,
3,3,3,3,3,3,3,3,3,3,3,3,3,3,3,3,3,3,3,3,3,3,3,3,3,3,3,3,3,3,3,3,3,3,3,3,
3,3,3,3,3,3,3,3,3,3,3,3,3,3,3,3,3,3,3,3,3,3,3,3,3,3,3,4),(-54.3584128772902,
-54.2562491996727,-54.1536641317825,-54.0508554030152,-53.9477257033755,
-53.9173311895702,-53.8220978553623,-53.726995864671,-53.6319956516206,
-53.5370639178197,-53.4421667036412,-53.347277449681,-53.2523696109718,
-53.1573574893496,-53.06228699457,-52.9670625627409,-52.918862093467,-52.8236288091345,
-52.7285268666147,-52.633526699971,-52.5385950097338,-52.4436978373347,
-52.3488086233097,-52.2539008226304,-52.1588887358914,-52.0638182742564,
-51.9685938725254,-51.9203929973639,-51.8251599103758,-51.7300581689489,
-51.6350582068426,-51.5401267254171,-51.4452297644054,-51.350340764085,
-51.2554331791706,-51.1604213100182,-51.0653510673298,-50.9701268845282,
-50.9219239012607,-50.826690702328,-50.7315888474202,-50.6365887704656,
-50.5416571726404,-50.4467600943099,-50.3518709758971,-50.2569632722615,
-50.1619512841573,-50.0668809222091,-49.9716566208346,-49.9234548051576,
-49.8282216195079,-49.7331197778338,-49.6381197140452,-49.5431881292274,
-49.4482910638008,-49.3534019581714,-49.2584942671821,-49.1634822914365,
-49.0684119417016,-48.9731876521932,-48.9249857090544,-48.8311534134105,
-48.7366626830585,-48.6430693691703,-48.5495338342124,-48.4560280787456,
-48.3608279517078,-48.2672557543579,-48.1712416624761,-48.0752275705943),
 .UNSPECIFIED.);
#158=B_SPLINE_CURVE_WITH_KNOTS('',3,(#16611,#16612,#16613,#16614,#16615,
#16616,#16617,#16618,#16619,#16620,#16621,#16622,#16623,#16624,#16625,#16626,
#16627,#16628,#16629,#16630,#16631,#16632,#16633,#16634,#16635,#16636,#16637,
#16638,#16639,#16640,#16641,#16642,#16643,#16644,#16645,#16646,#16647,#16648,
#16649,#16650,#16651,#16652,#16653,#16654,#16655,#16656,#16657,#16658,#16659,
#16660,#16661,#16662,#16663,#16664,#16665,#16666,#16667,#16668,#16669,#16670,
#16671,#16672,#16673,#16674,#16675,#16676,#16677,#16678,#16679,#16680,#16681,
#16682,#16683,#16684,#16685,#16686,#16687,#16688,#16689,#16690,#16691,#16692,
#16693,#16694,#16695,#16696,#16697,#16698,#16699,#16700,#16701,#16702,#16703,
#16704,#16705,#16706,#16707,#16708,#16709,#16710,#16711,#16712,#16713,#16714,
#16715,#16716,#16717,#16718,#16719,#16720,#16721,#16722,#16723,#16724,#16725,
#16726,#16727,#16728,#16729,#16730,#16731,#16732,#16733,#16734,#16735,#16736,
#16737,#16738,#16739,#16740,#16741,#16742,#16743,#16744,#16745,#16746,#16747,
#16748,#16749,#16750,#16751,#16752,#16753,#16754,#16755,#16756,#16757,#16758,
#16759,#16760,#16761,#16762,#16763,#16764,#16765,#16766,#16767,#16768,#16769,
#16770,#16771,#16772,#16773,#16774,#16775,#16776,#16777,#16778,#16779,#16780,
#16781,#16782,#16783,#16784,#16785,#16786,#16787,#16788,#16789,#16790,#16791,
#16792,#16793,#16794,#16795,#16796,#16797,#16798,#16799,#16800,#16801,#16802,
#16803,#16804,#16805,#16806,#16807,#16808,#16809,#16810,#16811,#16812,#16813,
#16814,#16815),.UNSPECIFIED.,.F.,.F.,(4,3,3,3,3,3,3,3,3,3,3,3,3,3,3,3,3,
3,3,3,3,3,3,3,3,3,3,3,3,3,3,3,3,3,3,3,3,3,3,3,3,3,3,3,3,3,3,3,3,3,3,3,3,
3,3,3,3,3,3,3,3,3,3,3,3,3,3,3,4),(-48.0752275703877,-47.9265166129513,-47.8312834332093,
-47.7361815976334,-47.6411815401237,-47.5462499618286,-47.4513529030737,
-47.356463804257,-47.2615561202136,-47.166544151575,-47.0714738090493,-46.9762495268394,
-46.9280475168481,-46.832814339316,-46.7377125059585,-46.6427124506726,
-46.5477808745998,-46.4528838180653,-46.3579947214643,-46.2630870396291,
-46.1680750731736,-46.07300473282,-45.9777804527437,-45.929578420745,-45.8343452448031,
-45.7392434130709,-45.6442433594427,-45.549311785069,-45.4544147302587,
-45.3595256354049,-45.2646179553379,-45.1696059906717,-45.0745356521221,
-44.9793113738549,-44.9311093246418,-44.8358761473955,-44.7407743143389,
-44.6457742593688,-44.5508426836322,-44.4559456274466,-44.3610565312069,
-44.2661488497449,-44.1711368836785,-44.0760665437236,-43.980842264057,
-43.9326402285387,-43.837407051605,-43.7423052188635,-43.6473051642101,
-43.5523735887918,-43.4574765329253,-43.3625874370049,-43.2676797558623,
-43.1726677901132,-43.0775974504749,-42.9823731711208,-42.9341711324355,
-42.8389379556324,-42.7438361230246,-42.6488360685081,-42.5539044932305,
-42.459007437507,-42.364118341732,-42.2692106607367,-42.174198695137,-42.0791283556497,
-41.9839040764474,-41.9357020363324,-41.792042263208),.UNSPECIFIED.);
#159=B_SPLINE_CURVE_WITH_KNOTS('',3,(#16817,#16818,#16819,#16820,#16821,
#16822,#16823,#16824,#16825,#16826,#16827,#16828,#16829,#16830,#16831,#16832,
#16833,#16834,#16835,#16836,#16837,#16838,#16839,#16840,#16841,#16842,#16843,
#16844,#16845,#16846,#16847,#16848,#16849,#16850,#16851,#16852,#16853,#16854,
#16855,#16856,#16857,#16858,#16859,#16860,#16861,#16862,#16863,#16864,#16865,
#16866,#16867,#16868,#16869,#16870,#16871,#16872,#16873,#16874,#16875,#16876,
#16877,#16878,#16879,#16880,#16881,#16882,#16883,#16884,#16885,#16886,#16887,
#16888,#16889,#16890,#16891,#16892,#16893,#16894,#16895,#16896,#16897,#16898,
#16899,#16900,#16901,#16902,#16903,#16904,#16905,#16906,#16907,#16908,#16909,
#16910,#16911,#16912,#16913,#16914,#16915,#16916,#16917,#16918,#16919,#16920,
#16921,#16922,#16923,#16924,#16925,#16926,#16927,#16928,#16929,#16930,#16931,
#16932,#16933,#16934,#16935,#16936,#16937,#16938,#16939,#16940,#16941,#16942,
#16943,#16944,#16945,#16946,#16947,#16948,#16949,#16950,#16951,#16952,#16953,
#16954,#16955,#16956,#16957,#16958,#16959,#16960,#16961,#16962,#16963,#16964,
#16965,#16966,#16967,#16968,#16969,#16970,#16971,#16972,#16973,#16974,#16975,
#16976,#16977,#16978,#16979,#16980,#16981,#16982,#16983,#16984,#16985,#16986,
#16987,#16988,#16989,#16990,#16991,#16992,#16993,#16994,#16995,#16996,#16997,
#16998,#16999,#17000,#17001,#17002,#17003,#17004,#17005,#17006,#17007,#17008,
#17009,#17010,#17011,#17012,#17013,#17014,#17015,#17016,#17017,#17018,#17019,
#17020,#17021,#17022,#17023,#17024),.UNSPECIFIED.,.F.,.F.,(4,3,3,3,3,3,
3,3,3,3,3,3,3,3,3,3,3,3,3,3,3,3,3,3,3,3,3,3,3,3,3,3,3,3,3,3,3,3,3,3,3,3,
3,3,3,3,3,3,3,3,3,3,3,3,3,3,3,3,3,3,3,3,3,3,3,3,3,3,3,4),(-41.7920422629959,
-41.6983020718591,-41.6031684304054,-41.5096071386079,-41.4160808478565,
-41.3225615994021,-41.2262294346088,-41.132586215821,-41.0349095780251,
-40.9372329402292,-40.8419997633305,-40.7468979306253,-40.6518978760097,
-40.5569663006309,-40.4620692448051,-40.3671801489268,-40.2722724678267,
-40.177260502122,-40.082190162529,-39.986965883221,-39.9387638441261,-39.8435306672368,
-39.7484288345412,-39.6534287799355,-39.5584972045672,-39.4636001487521,
-39.3687110528847,-39.2738033717959,-39.1787914061024,-39.0837210665206,
-38.9884967872241,-38.9402947480229,-38.8450615711197,-38.7499597384101,
-38.6549596837903,-38.5600281084075,-38.4651310525776,-38.3702419566952,
-38.2753342755915,-38.1803223098829,-38.0852519702858,-37.9900276909743,
-37.9418256519198,-37.8465924750215,-37.7514906423169,-37.6564905877022,
-37.5615590123245,-37.4666619564998,-37.3717728606225,-37.2768651795238,
-37.1818532138203,-37.0867828742286,-36.9915585949221,-36.9433565558166,
-36.8481233789189,-36.7530215462151,-36.6580214916009,-36.5630899162239,
-36.4681928603998,-36.373303764523,-36.2783960834249,-36.1833841177223,
-36.0883137781316,-35.9930894988259,-35.9448874597135,-35.8414187106333,
-35.7383353835895,-35.6355021233564,-35.5330254003549,-35.5088569563256),
 .UNSPECIFIED.);
#160=B_SPLINE_CURVE_WITH_KNOTS('',3,(#17026,#17027,#17028,#17029,#17030,
#17031,#17032,#17033,#17034,#17035,#17036,#17037,#17038,#17039,#17040,#17041,
#17042,#17043,#17044,#17045,#17046,#17047,#17048,#17049,#17050,#17051,#17052,
#17053,#17054,#17055,#17056,#17057,#17058,#17059,#17060,#17061,#17062,#17063,
#17064,#17065,#17066,#17067,#17068,#17069,#17070,#17071,#17072,#17073,#17074,
#17075,#17076,#17077,#17078,#17079,#17080,#17081,#17082,#17083,#17084,#17085,
#17086,#17087,#17088,#17089,#17090,#17091,#17092,#17093,#17094,#17095,#17096,
#17097,#17098,#17099,#17100,#17101,#17102,#17103,#17104,#17105,#17106,#17107,
#17108,#17109,#17110,#17111,#17112,#17113,#17114,#17115,#17116,#17117,#17118,
#17119,#17120,#17121,#17122,#17123,#17124,#17125,#17126,#17127,#17128,#17129,
#17130,#17131,#17132,#17133,#17134,#17135,#17136,#17137,#17138,#17139,#17140,
#17141,#17142,#17143,#17144,#17145,#17146,#17147,#17148,#17149,#17150,#17151,
#17152,#17153,#17154,#17155,#17156,#17157,#17158,#17159,#17160,#17161,#17162,
#17163,#17164,#17165,#17166,#17167,#17168,#17169,#17170,#17171,#17172,#17173,
#17174,#17175,#17176,#17177,#17178,#17179,#17180,#17181,#17182,#17183,#17184,
#17185,#17186,#17187,#17188,#17189,#17190,#17191,#17192,#17193,#17194,#17195,
#17196,#17197,#17198,#17199,#17200,#17201,#17202,#17203,#17204,#17205,#17206,
#17207,#17208,#17209,#17210,#17211,#17212,#17213,#17214,#17215,#17216,#17217,
#17218,#17219,#17220,#17221,#17222,#17223,#17224,#17225,#17226,#17227,#17228,
#17229,#17230,#17231,#17232,#17233),.UNSPECIFIED.,.F.,.F.,(4,3,3,3,3,3,
3,3,3,3,3,3,3,3,3,3,3,3,3,3,3,3,3,3,3,3,3,3,3,3,3,3,3,3,3,3,3,3,3,3,3,3,
3,3,3,3,3,3,3,3,3,3,3,3,3,3,3,3,3,3,3,3,3,3,3,3,3,3,3,4),(-35.5088569560286,
-35.4116942923171,-35.3144674214492,-35.2170727180144,-35.119590030636,
-35.0219006533429,-34.9464183636103,-34.8511851867119,-34.7560833540071,
-34.6610832993923,-34.5661517240144,-34.4712546681895,-34.3763655723121,
-34.2814578912133,-34.1864459255097,-34.0913755859181,-33.9961513066115,
-33.9479492675072,-33.8527160906088,-33.757614257904,-33.6626142032893,
-33.5676826279114,-33.4727855720865,-33.3778964762091,-33.2829887951106,
-33.1879768294071,-33.0929064898154,-32.9976822105088,-32.949480171404,
-32.8542469945053,-32.7591451618005,-32.6641451071851,-32.5692135318069,
-32.4743164759818,-32.3794273801041,-32.2845196990056,-32.1895077333018,
-32.09443739371,-31.9992131144032,-31.9510110753009,-31.8557778984026,-31.7606760656978,
-31.6656760110824,-31.5707444357045,-31.4758473798796,-31.3809582840021,
-31.2860506029035,-31.1910386372,-31.0959682976082,-31.0007440183016,-30.9525419791977,
-30.8573088022992,-30.7622069695944,-30.6672069149792,-30.5722753396014,
-30.4773782837763,-30.3824891878987,-30.2875815068003,-30.1925695410967,
-30.0974992015048,-30.0022749221982,-29.9540728830946,-29.8597759658973,
-29.7655993400692,-29.6715152517421,-29.5774960483942,-29.4834917361403,
-29.3894992479983,-29.2954458217341,-29.2256716488489),.UNSPECIFIED.);
#161=B_SPLINE_CURVE_WITH_KNOTS('',3,(#17235,#17236,#17237,#17238,#17239,
#17240,#17241,#17242,#17243,#17244,#17245,#17246,#17247,#17248,#17249,#17250,
#17251,#17252,#17253,#17254,#17255,#17256,#17257,#17258,#17259,#17260,#17261,
#17262,#17263,#17264,#17265,#17266,#17267,#17268,#17269,#17270,#17271,#17272,
#17273,#17274,#17275,#17276,#17277,#17278,#17279,#17280,#17281,#17282,#17283,
#17284,#17285,#17286,#17287,#17288,#17289,#17290,#17291,#17292,#17293,#17294,
#17295,#17296,#17297,#17298,#17299,#17300,#17301,#17302,#17303,#17304,#17305,
#17306,#17307,#17308,#17309,#17310,#17311,#17312,#17313,#17314,#17315,#17316,
#17317,#17318,#17319,#17320,#17321,#17322,#17323,#17324,#17325,#17326,#17327,
#17328,#17329,#17330,#17331,#17332,#17333,#17334,#17335,#17336,#17337,#17338,
#17339,#17340,#17341,#17342,#17343,#17344,#17345,#17346,#17347,#17348,#17349,
#17350,#17351,#17352,#17353,#17354,#17355,#17356,#17357,#17358,#17359,#17360,
#17361,#17362,#17363,#17364,#17365,#17366,#17367,#17368,#17369,#17370,#17371,
#17372,#17373,#17374,#17375,#17376,#17377,#17378,#17379,#17380,#17381,#17382,
#17383,#17384,#17385,#17386,#17387,#17388,#17389,#17390,#17391,#17392,#17393,
#17394,#17395,#17396,#17397,#17398,#17399,#17400,#17401,#17402,#17403,#17404,
#17405,#17406,#17407,#17408,#17409,#17410,#17411,#17412,#17413,#17414,#17415,
#17416,#17417,#17418,#17419,#17420,#17421,#17422,#17423,#17424,#17425,#17426,
#17427,#17428,#17429,#17430,#17431,#17432,#17433,#17434,#17435,#17436,#17437,
#17438,#17439,#17440,#17441,#17442,#17443,#17444,#17445),.UNSPECIFIED.,
 .F.,.F.,(4,3,3,3,3,3,3,3,3,3,3,3,3,3,3,3,3,3,3,3,3,3,3,3,3,3,3,3,3,3,3,
3,3,3,3,3,3,3,3,3,3,3,3,3,3,3,3,3,3,3,3,3,3,3,3,3,3,3,3,3,3,3,3,3,3,3,3,
3,3,3,4),(-29.2256716486763,-29.1072434664186,-28.986625190017,-28.9556037869914,
-28.8603706100939,-28.76526877739,-28.6702687227759,-28.5753371473988,-28.4804400915747,
-28.3855509956981,-28.2906433146002,-28.1956313488974,-28.1005610093064,
-28.0053367300007,-27.9571346908882,-27.86190151399,-27.7667996812855,-27.6717996266707,
-27.576868051293,-27.4819709954682,-27.387081899591,-27.2921742184927,-27.1971622527894,
-27.1020919131979,-27.0068676338916,-26.9586655947851,-26.8634324178817,
-26.768330585172,-26.6733305305519,-26.578398955169,-26.483501899339,-26.3886128034566,
-26.293705122353,-26.1986931566446,-26.1036228170479,-26.0083985377366,
-25.9601964986819,-25.8649633217936,-25.769861489099,-25.674861434494,-25.579929859126,
-25.485032803311,-25.3901437074434,-25.2952360263545,-25.2002240606605,
-25.1051537210782,-25.0099294417809,-24.9617274025788,-24.8664942256789,
-24.7713923929728,-24.6763923383566,-24.5814607629776,-24.4865637071516,
-24.3916746112732,-24.2967669301737,-24.2017549644695,-24.1066846248772,
-24.0114603455702,-23.9632583064756,-23.8680251295345,-23.7729232967871,
-23.6779232421291,-23.5829916667083,-23.4880946108405,-23.3932055149203,
-23.298297833779,-23.2032858680333,-23.1082155283996,-23.0129912490518,
-22.9647892103725,-22.9424863416694),.UNSPECIFIED.);
#162=B_SPLINE_CURVE_WITH_KNOTS('',3,(#17447,#17448,#17449,#17450,#17451,
#17452,#17453,#17454,#17455,#17456,#17457,#17458,#17459,#17460,#17461,#17462,
#17463,#17464,#17465,#17466,#17467,#17468,#17469,#17470,#17471,#17472,#17473,
#17474,#17475,#17476,#17477,#17478,#17479,#17480,#17481,#17482,#17483,#17484,
#17485,#17486,#17487,#17488,#17489,#17490,#17491,#17492,#17493,#17494,#17495,
#17496,#17497,#17498,#17499,#17500,#17501,#17502,#17503,#17504,#17505,#17506,
#17507,#17508,#17509,#17510,#17511,#17512,#17513,#17514,#17515,#17516,#17517,
#17518,#17519,#17520,#17521,#17522,#17523,#17524,#17525,#17526,#17527,#17528,
#17529,#17530,#17531,#17532,#17533,#17534,#17535,#17536,#17537,#17538,#17539,
#17540,#17541,#17542,#17543,#17544,#17545,#17546,#17547,#17548,#17549,#17550,
#17551,#17552,#17553,#17554,#17555,#17556,#17557,#17558,#17559,#17560,#17561,
#17562,#17563,#17564,#17565,#17566,#17567,#17568,#17569,#17570,#17571,#17572,
#17573,#17574,#17575,#17576,#17577,#17578,#17579,#17580,#17581,#17582,#17583,
#17584,#17585,#17586,#17587,#17588,#17589,#17590,#17591,#17592,#17593,#17594,
#17595,#17596,#17597,#17598,#17599,#17600,#17601,#17602,#17603,#17604,#17605,
#17606,#17607,#17608,#17609,#17610,#17611,#17612,#17613,#17614,#17615,#17616,
#17617,#17618,#17619,#17620,#17621,#17622,#17623,#17624,#17625,#17626,#17627,
#17628,#17629,#17630,#17631,#17632,#17633,#17634,#17635,#17636,#17637,#17638,
#17639,#17640,#17641,#17642,#17643,#17644,#17645,#17646,#17647,#17648,#17649,
#17650,#17651,#17652,#17653,#17654),.UNSPECIFIED.,.F.,.F.,(4,3,3,3,3,3,
3,3,3,3,3,3,3,3,3,3,3,3,3,3,3,3,3,3,3,3,3,3,3,3,3,3,3,3,3,3,3,3,3,3,3,3,
3,3,3,3,3,3,3,3,3,3,3,3,3,3,3,3,3,3,3,3,3,3,3,3,3,3,3,4),(-22.942486341331,
-22.8476150237653,-22.7528740368907,-22.654554796563,-22.5599818052167,
-22.4654400589883,-22.3709025735227,-22.2763423756061,-22.1816765680522,
-22.086947869278,-21.9920723020764,-21.9663201142693,-21.8710869373234,
-21.7759851045722,-21.6809850499115,-21.5860534744897,-21.491156418622,
-21.3962673227029,-21.3013596415636,-21.2063476758215,-21.1112773361922,
-21.01605305685,-20.9678510181662,-20.8726178409093,-20.7775160078446,-20.6825159528683,
-20.5875843771288,-20.4926873209421,-20.3977982247034,-20.3028905432446,
-20.2078785771841,-20.1128082372368,-20.0175839575806,-19.969381922063,
-19.8741487462001,-19.7790469145306,-19.6840468609492,-19.5891152865979,
-19.494218231795,-19.3993291369339,-19.3044214568442,-19.2094094921331,
-19.1143391535259,-19.0191148751815,-18.9709128259599,-18.8756796482935,
-18.7805778148294,-18.6855777594645,-18.5906461833534,-18.4957491268059,
-18.4008600302176,-18.3059523484206,-18.2109403820415,-18.115870041786,
-18.0206457618408,-17.9724437298567,-17.877210550068,-17.7821087144555,
-17.6871086569185,-17.5921770786102,-17.4972800198508,-17.4023909210385,
-17.3074832370082,-17.2124712683962,-17.1174009259047,-17.0221766437404,
-16.9739746337536,-16.8599445077596,-16.7472092989469,-16.6593010346695),
 .UNSPECIFIED.);
#163=B_SPLINE_CURVE_WITH_KNOTS('',3,(#17656,#17657,#17658,#17659,#17660,
#17661,#17662,#17663,#17664,#17665,#17666,#17667,#17668,#17669,#17670,#17671,
#17672,#17673,#17674,#17675,#17676,#17677,#17678,#17679,#17680,#17681,#17682,
#17683,#17684,#17685,#17686,#17687,#17688,#17689,#17690,#17691,#17692,#17693,
#17694,#17695,#17696,#17697,#17698,#17699,#17700,#17701,#17702,#17703,#17704,
#17705,#17706,#17707,#17708,#17709,#17710,#17711,#17712,#17713,#17714,#17715,
#17716,#17717,#17718,#17719,#17720,#17721,#17722,#17723,#17724,#17725,#17726,
#17727,#17728,#17729,#17730,#17731,#17732,#17733,#17734,#17735,#17736,#17737,
#17738,#17739,#17740,#17741,#17742,#17743,#17744,#17745,#17746,#17747,#17748,
#17749,#17750,#17751,#17752,#17753,#17754,#17755,#17756,#17757,#17758,#17759,
#17760,#17761,#17762,#17763,#17764,#17765,#17766,#17767,#17768,#17769,#17770,
#17771,#17772,#17773,#17774,#17775,#17776,#17777,#17778,#17779,#17780,#17781,
#17782,#17783,#17784,#17785,#17786,#17787,#17788,#17789,#17790,#17791,#17792,
#17793,#17794,#17795,#17796,#17797,#17798,#17799,#17800,#17801,#17802,#17803,
#17804,#17805,#17806,#17807,#17808,#17809,#17810,#17811,#17812,#17813,#17814,
#17815,#17816,#17817,#17818,#17819,#17820,#17821,#17822,#17823,#17824,#17825,
#17826,#17827,#17828,#17829,#17830,#17831,#17832,#17833,#17834,#17835,#17836,
#17837,#17838,#17839,#17840,#17841,#17842,#17843,#17844,#17845,#17846,#17847,
#17848,#17849,#17850,#17851,#17852,#17853,#17854,#17855,#17856,#17857,#17858,
#17859,#17860,#17861,#17862,#17863,#17864,#17865,#17866),.UNSPECIFIED.,
 .F.,.F.,(4,3,3,3,3,3,3,3,3,3,3,3,3,3,3,3,3,3,3,3,3,3,3,3,3,3,3,3,3,3,3,
3,3,3,3,3,3,3,3,3,3,3,3,3,3,3,3,3,3,3,3,3,3,3,3,3,3,3,3,3,3,3,3,3,3,3,3,
3,3,3,4),(-16.6593010344898,-16.564737636787,-16.4701999869256,-16.3756611684414,
-16.281094271255,-16.1864152516017,-16.0916687801366,-15.9967719690251,
-15.9755055376504,-15.8802723505797,-15.7851705077762,-15.6901704431488,
-15.5952388579267,-15.5003417923652,-15.4054526868703,-15.3105449962849,
-15.2155330213483,-15.1204626726541,-15.0252383845358,-14.9770364415473,
-14.8818032426871,-14.7867013878369,-14.691701310925,-14.5967697131203,
-14.5018726347967,-14.406983516377,-14.3120758127208,-14.2170638245753,
-14.121993462574,-14.0267691611285,-13.9785673454441,-13.8833342646743,
-13.7882325281889,-13.6932325697527,-13.5983010900969,-13.5034041296754,
-13.4085151287669,-13.3136075420861,-13.2185956693933,-13.123525422151,
-13.028301233267,-12.980098249341,-12.8848649504053,-12.7897629962807,-12.6947628210174,
-12.5998311266244,-12.5049339528391,-12.4100447401951,-12.3151369436636,
-12.2201248652386,-12.1250544142982,-12.0298300268517,-11.9816291532378,
-11.8863958246192,-11.7912938383692,-11.6962936286177,-11.6013618964074,
-11.5064646827596,-11.411575428271,-11.3166675879739,-11.2216554631697,
-11.1265849642967,-11.0313605270005,-10.9831600571347,-10.88673590317,-10.7904530193315,
-10.6942866233368,-10.5982246406379,-10.5022232640172,-10.4062551289695,
-10.3761157273101),.UNSPECIFIED.);
#164=B_SPLINE_CURVE_WITH_KNOTS('',3,(#17868,#17869,#17870,#17871,#17872,
#17873,#17874,#17875,#17876,#17877,#17878,#17879,#17880,#17881,#17882,#17883,
#17884,#17885,#17886,#17887,#17888,#17889,#17890,#17891,#17892,#17893,#17894,
#17895,#17896,#17897,#17898,#17899,#17900,#17901,#17902,#17903,#17904,#17905,
#17906,#17907,#17908,#17909,#17910,#17911,#17912,#17913,#17914,#17915,#17916,
#17917,#17918,#17919,#17920,#17921,#17922,#17923,#17924,#17925,#17926,#17927,
#17928,#17929,#17930,#17931,#17932,#17933,#17934,#17935,#17936,#17937,#17938,
#17939,#17940,#17941,#17942,#17943,#17944,#17945,#17946,#17947,#17948,#17949,
#17950,#17951,#17952,#17953,#17954,#17955,#17956,#17957,#17958,#17959,#17960,
#17961,#17962,#17963,#17964,#17965,#17966,#17967,#17968,#17969,#17970,#17971,
#17972,#17973,#17974,#17975,#17976,#17977,#17978,#17979,#17980,#17981,#17982,
#17983,#17984,#17985,#17986,#17987,#17988,#17989,#17990,#17991,#17992,#17993,
#17994,#17995,#17996,#17997,#17998,#17999,#18000,#18001,#18002,#18003,#18004,
#18005,#18006,#18007,#18008,#18009,#18010,#18011,#18012,#18013,#18014,#18015,
#18016,#18017,#18018,#18019,#18020,#18021,#18022,#18023,#18024,#18025,#18026,
#18027,#18028,#18029,#18030,#18031,#18032,#18033,#18034,#18035,#18036,#18037,
#18038,#18039,#18040,#18041,#18042,#18043,#18044,#18045,#18046,#18047,#18048,
#18049,#18050,#18051,#18052,#18053,#18054,#18055,#18056,#18057,#18058,#18059,
#18060,#18061,#18062,#18063,#18064,#18065,#18066,#18067,#18068,#18069,#18070,
#18071,#18072,#18073,#18074,#18075),.UNSPECIFIED.,.F.,.F.,(4,3,3,3,3,3,
3,3,3,3,3,3,3,3,3,3,3,3,3,3,3,3,3,3,3,3,3,3,3,3,3,3,3,3,3,3,3,3,3,3,3,3,
3,3,3,3,3,3,3,3,3,3,3,3,3,3,3,3,3,3,3,3,3,3,3,3,3,3,3,4),(-10.3761157271004,
-10.2705941373572,-10.1646889495115,-10.0582504347146,-9.98469096103152,
-9.88945640702594,-9.79435320216464,-9.69935178211476,-9.60441885682833,
-9.50952046120628,-9.41463003723521,-9.31972104134926,-9.22470778890569,
-9.12963617659603,-9.03441065868313,-8.98622186492837,-8.89098782101992,
-8.79588510357613,-8.70088414794559,-8.60595165136803,-8.51105366220213,
-8.41616362207912,-8.32125498705802,-8.22624205877446,-8.13117075025981,
-8.03594550181371,-7.98775276882521,-7.89252776793133,-7.79743412964125,
-7.70244227657632,-7.60751887932103,-7.51262998407767,-7.41774902126599,
-7.32284943571592,-7.22784545952439,-7.13278306108336,-7.03756657027433,
-6.98928367272206,-6.8940356024099,-6.79891891365831,-6.70390405982608,
-6.6089578300529,-6.51404621497145,-6.41914267241841,-6.32422067476947,
-6.22919467579913,-6.13411044309066,-6.03887262308352,-5.99081457661891,
-5.89557879637505,-5.80047419276722,-5.70547120593688,-5.61053647357262,
-5.51563612290772,-5.42074359936495,-5.32583236269098,-5.2308166714205,
-5.13574250420529,-5.04051427801215,-4.99234548051576,-4.89835863124272,
-4.80450220502569,-4.71075270953591,-4.6170611967346,-4.52339979495569,
-4.4297406695336,-4.33600307487336,-4.24222301883573,-4.14830479318644,
-4.09293042036874),.UNSPECIFIED.);
#165=B_SPLINE_CURVE_WITH_KNOTS('',3,(#18077,#18078,#18079,#18080,#18081,
#18082,#18083,#18084,#18085,#18086,#18087,#18088,#18089,#18090,#18091,#18092,
#18093,#18094,#18095,#18096,#18097,#18098,#18099,#18100,#18101,#18102,#18103,
#18104,#18105,#18106,#18107,#18108,#18109,#18110,#18111,#18112,#18113,#18114,
#18115,#18116,#18117,#18118,#18119,#18120,#18121,#18122,#18123,#18124,#18125,
#18126,#18127,#18128,#18129,#18130,#18131,#18132,#18133,#18134,#18135,#18136,
#18137,#18138,#18139,#18140,#18141,#18142,#18143),.UNSPECIFIED.,.F.,.F.,
(4,3,3,3,3,3,3,3,3,3,3,3,3,3,3,3,3,3,3,3,3,3,4),(-4.09293042013064,-3.99387638441261,
-3.89848924053276,-3.80323366876535,-3.70808031071437,-3.61299671406167,
-3.51794849283965,-3.4229092732933,-3.32785269704006,-3.23269459728435,
-3.13747948209115,-3.04211393352018,-2.99540728830946,-2.90121559909012,
-2.80715256457177,-2.7131934050502,-2.61929079818114,-2.52541705715098,
-2.43154452959619,-2.3375858729544,-2.24358441504212,-2.14942728251797,
-2.06864179208665),.UNSPECIFIED.);
#166=B_SPLINE_CURVE_WITH_KNOTS('',3,(#18144,#18145,#18146,#18147),
 .UNSPECIFIED.,.F.,.F.,(4,4),(-0.0553882262895087,0.),.UNSPECIFIED.);
#167=B_SPLINE_CURVE_WITH_KNOTS('',3,(#18150,#18151,#18152,#18153,#18154,
#18155,#18156,#18157,#18158,#18159,#18160,#18161,#18162,#18163,#18164,#18165,
#18166,#18167,#18168,#18169,#18170,#18171,#18172,#18173,#18174,#18175,#18176,
#18177,#18178,#18179,#18180,#18181,#18182,#18183,#18184,#18185,#18186,#18187,
#18188,#18189,#18190,#18191,#18192,#18193,#18194,#18195,#18196,#18197,#18198,
#18199,#18200,#18201,#18202,#18203,#18204,#18205,#18206,#18207,#18208,#18209,
#18210,#18211,#18212,#18213,#18214,#18215,#18216,#18217,#18218,#18219,#18220,
#18221,#18222,#18223,#18224,#18225,#18226,#18227,#18228,#18229,#18230,#18231,
#18232,#18233,#18234,#18235,#18236,#18237,#18238,#18239,#18240,#18241,#18242,
#18243,#18244,#18245,#18246,#18247,#18248,#18249,#18250,#18251,#18252,#18253,
#18254,#18255,#18256,#18257,#18258,#18259,#18260,#18261,#18262,#18263,#18264,
#18265),.UNSPECIFIED.,.F.,.F.,(4,2,2,2,2,2,2,2,2,2,2,2,2,2,2,2,2,2,2,2,
2,2,2,2,2,2,2,2,2,2,2,2,2,2,2,2,2,2,2,2,2,2,2,2,2,2,2,2,2,2,2,2,2,2,2,2,
2,4),(0.00393879945399954,0.0559409183588363,0.0876972450261331,0.0976998745863839,
0.104613482977544,0.11166922140705,0.122434269394492,0.179131978558203,
0.210354110329382,0.216991056490599,0.221067292598832,0.225123889707987,
0.231759555487665,0.261970513582465,0.302284660286109,0.325250128468266,
0.334362352316371,0.341123207111329,0.348441239547103,0.360557058247711,
0.406262420026052,0.434559681824057,0.450020364199544,0.45554426629461,
0.459375550971286,0.463708309240328,0.471808681292075,0.502901677971822,
0.532030064578008,0.561159612056953,0.570874880434037,0.577678874304539,
0.583863827512892,0.593949037105209,0.625063658570325,0.661425587696632,
0.686059983943537,0.69235077777511,0.696301740721866,0.700359261123135,
0.707095866720147,0.743137023178607,0.777207886595307,0.800425351770403,
0.809544959571145,0.81628096716921,0.823541975926377,0.835486602649266,
0.883868277417384,0.910317304618082,0.925173636210761,0.930612516942996,
0.934428206452051,0.938813273964349,0.946886601823189,0.978921547363476,
1.00811846899774,1.00824602608924),.UNSPECIFIED.);
#168=B_SPLINE_CURVE_WITH_KNOTS('',3,(#18269,#18270,#18271,#18272,#18273,
#18274,#18275,#18276,#18277,#18278,#18279,#18280,#18281,#18282,#18283,#18284,
#18285,#18286,#18287,#18288,#18289,#18290,#18291,#18292,#18293,#18294,#18295,
#18296,#18297,#18298,#18299),.UNSPECIFIED.,.F.,.F.,(4,3,3,3,3,3,3,3,3,3,
4),(72.2566310328722,72.358764204796,72.4649147790848,72.5667140368636,
72.6684219268066,72.7700668437146,72.8716771107077,72.973313692877,73.0749655043999,
73.1767014162145,73.207968799106),.UNSPECIFIED.);
#169=B_SPLINE_CURVE_WITH_KNOTS('',3,(#18300,#18301,#18302,#18303,#18304,
#18305,#18306,#18307,#18308,#18309,#18310,#18311,#18312,#18313,#18314,#18315,
#18316,#18317,#18318,#18319,#18320,#18321,#18322,#18323,#18324,#18325,#18326,
#18327,#18328,#18329,#18330,#18331,#18332,#18333,#18334,#18335,#18336,#18337,
#18338,#18339,#18340,#18341,#18342,#18343,#18344,#18345,#18346,#18347,#18348,
#18349,#18350,#18351,#18352,#18353,#18354,#18355,#18356,#18357,#18358,#18359,
#18360,#18361,#18362,#18363,#18364,#18365,#18366),.UNSPECIFIED.,.F.,.F.,
(4,3,3,3,3,3,3,3,3,3,3,3,3,3,3,3,3,3,3,3,3,3,4),(70.2101735890481,70.2125615107965,
70.3130249063546,70.413345018932,70.5135515181276,70.6136960857837,70.7138100121525,
70.813924548465,70.9141425502769,71.0144104356228,71.1148647428971,71.2110306068997,
71.3108636815101,71.4105510300929,71.5104196142066,71.6099303183161,71.7094110548427,
71.8088939006647,71.9090453512492,72.0086912716984,72.1090954873506,72.2094997030028,
72.2566310325651),.UNSPECIFIED.);
#170=B_SPLINE_CURVE_WITH_KNOTS('',3,(#18639,#18640,#18641,#18642,#18643,
#18644,#18645,#18646,#18647,#18648,#18649,#18650,#18651,#18652,#18653,#18654,
#18655,#18656,#18657,#18658,#18659,#18660,#18661,#18662,#18663,#18664,#18665,
#18666,#18667,#18668,#18669,#18670,#18671,#18672,#18673,#18674,#18675,#18676,
#18677,#18678,#18679,#18680,#18681,#18682,#18683,#18684,#18685,#18686,#18687,
#18688,#18689,#18690,#18691,#18692,#18693,#18694,#18695,#18696,#18697,#18698,
#18699,#18700,#18701,#18702,#18703,#18704,#18705,#18706,#18707,#18708,#18709,
#18710,#18711,#18712,#18713,#18714,#18715,#18716,#18717,#18718,#18719,#18720,
#18721,#18722,#18723,#18724,#18725,#18726,#18727,#18728,#18729,#18730,#18731,
#18732),.UNSPECIFIED.,.F.,.F.,(4,3,3,3,3,3,3,3,3,3,3,3,3,3,3,3,3,3,3,3,
3,3,3,3,3,3,3,3,3,3,3,4),(0.,0.0211515250929699,0.0503479224047965,0.0799219030506932,
0.107557403668628,0.112306557576265,0.116555306404556,0.145320497988993,
0.173988624024303,0.202002260365531,0.214552337294273,0.219717600821093,
0.223840641427237,0.251416480277754,0.27821193354047,0.301838152182752,
0.317677816946291,0.324502722029292,0.329013266588695,0.3558249978195,0.382923040397653,
0.405945422486999,0.417986286650722,0.424997553960968,0.429588563398635,
0.455730667603274,0.480731501813387,0.487617912295433,0.494575057586814,
0.519602150133133,0.544372461559281,0.555272788399386),.UNSPECIFIED.);
#171=B_SPLINE_CURVE_WITH_KNOTS('',3,(#18733,#18734,#18735,#18736,#18737,
#18738,#18739,#18740,#18741,#18742,#18743,#18744,#18745,#18746,#18747,#18748,
#18749,#18750,#18751,#18752,#18753,#18754,#18755,#18756,#18757,#18758,#18759,
#18760,#18761,#18762,#18763,#18764,#18765,#18766,#18767,#18768,#18769,#18770,
#18771,#18772,#18773,#18774,#18775,#18776,#18777,#18778,#18779,#18780,#18781,
#18782,#18783,#18784,#18785,#18786,#18787,#18788,#18789,#18790,#18791,#18792,
#18793,#18794,#18795,#18796,#18797,#18798,#18799,#18800,#18801,#18802,#18803,
#18804,#18805,#18806,#18807,#18808,#18809,#18810,#18811,#18812,#18813,#18814,
#18815,#18816,#18817,#18818,#18819,#18820),.UNSPECIFIED.,.F.,.F.,(4,3,3,
3,3,3,3,3,3,3,3,3,3,3,3,3,3,3,3,3,3,3,3,3,3,3,3,3,3,4),(-0.555272788399294,
-0.537998135235996,-0.513195393070161,-0.498873792586909,-0.492711473426493,
-0.487860772154604,-0.462111258555471,-0.439632717483603,-0.428896962458095,
-0.424839679808983,-0.398150918614796,-0.371100690967241,-0.344106017964823,
-0.328877992852833,-0.32454079642153,-0.296627170519809,-0.282566212897678,
-0.255355425971256,-0.228144639044835,-0.22107377310443,-0.216711755873243,
-0.188903627081518,-0.160211248623033,-0.131518870164547,-0.114266101543064,
-0.109583468965517,-0.0801051988652096,-0.0505616879768782,-0.0216028909587886,
0.),.UNSPECIFIED.);
#172=B_SPLINE_CURVE_WITH_KNOTS('',3,(#18822,#18823,#18824,#18825,#18826,
#18827,#18828,#18829,#18830,#18831,#18832,#18833,#18834,#18835,#18836,#18837,
#18838,#18839,#18840,#18841,#18842,#18843,#18844,#18845,#18846,#18847,#18848,
#18849,#18850,#18851,#18852,#18853,#18854,#18855,#18856,#18857,#18858,#18859,
#18860,#18861,#18862,#18863,#18864,#18865,#18866,#18867,#18868,#18869,#18870,
#18871,#18872,#18873,#18874,#18875,#18876,#18877,#18878,#18879,#18880,#18881,
#18882,#18883,#18884,#18885,#18886,#18887,#18888,#18889,#18890,#18891,#18892,
#18893,#18894,#18895,#18896,#18897,#18898,#18899,#18900,#18901,#18902,#18903,
#18904,#18905,#18906,#18907,#18908,#18909,#18910,#18911,#18912,#18913,#18914,
#18915),.UNSPECIFIED.,.F.,.F.,(4,3,3,3,3,3,3,3,3,3,3,3,3,3,3,3,3,3,3,3,
3,3,3,3,3,3,3,3,3,3,3,4),(-0.547176240833745,-0.531693267680898,-0.502322832918406,
-0.486713217316651,-0.479140335200163,-0.472082504350801,-0.44303092644762,
-0.419220841452745,-0.408408989901447,-0.402036527603242,-0.397475090495561,
-0.369198891406047,-0.341216278386301,-0.314050980020528,-0.297439627272632,
-0.29142916710721,-0.264617850724684,-0.252568983290324,-0.224809796970208,
-0.197050610650091,-0.192202487211981,-0.188184385718677,-0.161573441667812,
-0.135063262774347,-0.108787981383092,-0.0997862447992211,-0.0945269665459779,
-0.0902272799954171,-0.064692601081796,-0.039564031532061,-0.0152229077075751,
0.),.UNSPECIFIED.);
#173=B_SPLINE_CURVE_WITH_KNOTS('',3,(#19189,#19190,#19191,#19192,#19193,
#19194,#19195,#19196,#19197,#19198,#19199,#19200,#19201,#19202,#19203,#19204,
#19205,#19206,#19207,#19208,#19209,#19210,#19211,#19212,#19213,#19214,#19215,
#19216,#19217,#19218,#19219,#19220,#19221,#19222,#19223,#19224,#19225,#19226,
#19227,#19228,#19229,#19230,#19231,#19232,#19233,#19234,#19235,#19236,#19237,
#19238,#19239,#19240,#19241,#19242,#19243,#19244,#19245,#19246,#19247,#19248,
#19249,#19250,#19251,#19252,#19253,#19254,#19255,#19256,#19257,#19258,#19259,
#19260,#19261,#19262,#19263,#19264,#19265,#19266,#19267,#19268,#19269,#19270,
#19271,#19272,#19273,#19274,#19275,#19276,#19277,#19278,#19279),
 .UNSPECIFIED.,.F.,.F.,(4,3,3,3,3,3,3,3,3,3,3,3,3,3,3,3,3,3,3,3,3,3,3,3,
3,3,3,3,3,3,4),(0.,0.0172144967118733,0.041750612664055,0.0670931170711941,
0.0923753317934749,0.0966923746148899,0.122587060977129,0.149199398849806,
0.175811736722484,0.187831472308839,0.191843178428869,0.196232750464077,
0.223664672674057,0.251007710322057,0.271753036768803,0.289315058119197,
0.293959260700982,0.29839462330624,0.326041543022183,0.353688462738127,
0.37857057719275,0.391580430417787,0.398055686999867,0.403828921411263,
0.433238481825865,0.462648042240467,0.472327168294413,0.47934658435098,
0.508876613490308,0.538109240394632,0.55274537837511),.UNSPECIFIED.);
#174=B_SPLINE_CURVE_WITH_KNOTS('',3,(#19280,#19281,#19282,#19283),
 .UNSPECIFIED.,.F.,.F.,(4,4),(0.,0.0136660632777819),.UNSPECIFIED.);
#175=SHAPE_REPRESENTATION_RELATIONSHIP('SRR','None',#19475,#183);
#176=SHAPE_REPRESENTATION_RELATIONSHIP('SRR','None',#19476,#184);
#177=SHAPE_REPRESENTATION_RELATIONSHIP('SRR','None',#19477,#185);
#178=SHAPE_REPRESENTATION_RELATIONSHIP('SRR','None',#19478,#186);
#179=SHAPE_REPRESENTATION_RELATIONSHIP('SRR','None',#19479,#187);
#180=SHAPE_REPRESENTATION_RELATIONSHIP('SRR','None',#19480,#188);
#181=SHAPE_REPRESENTATION_RELATIONSHIP('SRR','None',#19481,#189);
#182=SHAPE_REPRESENTATION_RELATIONSHIP('SRR','None',#19482,#190);
#183=ADVANCED_BREP_SHAPE_REPRESENTATION('',(#199),#19435);
#184=ADVANCED_BREP_SHAPE_REPRESENTATION('',(#200),#19436);
#185=ADVANCED_BREP_SHAPE_REPRESENTATION('',(#201),#19437);
#186=ADVANCED_BREP_SHAPE_REPRESENTATION('',(#202),#19438);
#187=ADVANCED_BREP_SHAPE_REPRESENTATION('',(#203),#19439);
#188=ADVANCED_BREP_SHAPE_REPRESENTATION('',(#204),#19440);
#189=ADVANCED_BREP_SHAPE_REPRESENTATION('',(#205),#19441);
#190=ADVANCED_BREP_SHAPE_REPRESENTATION('',(#206),#19442);
#191=STYLED_ITEM('',(#19524),#199);
#192=STYLED_ITEM('',(#19524),#200);
#193=STYLED_ITEM('',(#19524),#201);
#194=STYLED_ITEM('',(#19525),#202);
#195=STYLED_ITEM('',(#19525),#203);
#196=STYLED_ITEM('',(#19525),#204);
#197=STYLED_ITEM('',(#19525),#205);
#198=STYLED_ITEM('',(#19525),#206);
#199=MANIFOLD_SOLID_BREP('Body1',#2018);
#200=MANIFOLD_SOLID_BREP('Body1',#2019);
#201=MANIFOLD_SOLID_BREP('Body1',#2020);
#202=MANIFOLD_SOLID_BREP('Body1',#2021);
#203=MANIFOLD_SOLID_BREP('Body1',#2022);
#204=MANIFOLD_SOLID_BREP('Body1',#2023);
#205=MANIFOLD_SOLID_BREP('Body1',#2024);
#206=MANIFOLD_SOLID_BREP('Body1',#2025);
#207=FACE_BOUND('',#372,.T.);
#208=FACE_BOUND('',#374,.T.);
#209=FACE_BOUND('',#387,.T.);
#210=FACE_BOUND('',#410,.T.);
#211=FACE_BOUND('',#414,.T.);
#212=FACE_BOUND('',#420,.T.);
#213=FACE_BOUND('',#427,.T.);
#214=FACE_BOUND('',#439,.T.);
#215=FACE_BOUND('',#445,.T.);
#216=FACE_BOUND('',#457,.T.);
#217=FACE_BOUND('',#459,.T.);
#218=FACE_BOUND('',#475,.T.);
#219=FACE_BOUND('',#477,.T.);
#220=PLANE('',#2123);
#221=PLANE('',#2124);
#222=PLANE('',#2129);
#223=PLANE('',#2130);
#224=PLANE('',#2147);
#225=PLANE('',#2148);
#226=PLANE('',#2149);
#227=PLANE('',#2154);
#228=PLANE('',#2158);
#229=PLANE('',#2159);
#230=PLANE('',#2160);
#231=PLANE('',#2161);
#232=PLANE('',#2162);
#233=PLANE('',#2163);
#234=PLANE('',#2164);
#235=PLANE('',#2165);
#236=PLANE('',#2166);
#237=PLANE('',#2167);
#238=PLANE('',#2168);
#239=PLANE('',#2172);
#240=PLANE('',#2173);
#241=PLANE('',#2174);
#242=PLANE('',#2181);
#243=PLANE('',#2182);
#244=PLANE('',#2186);
#245=PLANE('',#2187);
#246=PLANE('',#2194);
#247=PLANE('',#2213);
#248=PLANE('',#2214);
#249=PLANE('',#2218);
#250=PLANE('',#2219);
#251=PLANE('',#2224);
#252=PLANE('',#2225);
#253=PLANE('',#2226);
#254=PLANE('',#2227);
#255=PLANE('',#2228);
#256=PLANE('',#2229);
#257=PLANE('',#2230);
#258=PLANE('',#2231);
#259=PLANE('',#2233);
#260=PLANE('',#2235);
#261=PLANE('',#2237);
#262=PLANE('',#2239);
#263=PLANE('',#2244);
#264=PLANE('',#2245);
#265=PLANE('',#2250);
#266=PLANE('',#2251);
#267=PLANE('',#2252);
#268=PLANE('',#2253);
#269=PLANE('',#2254);
#270=PLANE('',#2255);
#271=PLANE('',#2256);
#272=PLANE('',#2257);
#273=FACE_OUTER_BOUND('',#369,.T.);
#274=FACE_OUTER_BOUND('',#370,.T.);
#275=FACE_OUTER_BOUND('',#371,.T.);
#276=FACE_OUTER_BOUND('',#373,.T.);
#277=FACE_OUTER_BOUND('',#375,.T.);
#278=FACE_OUTER_BOUND('',#376,.T.);
#279=FACE_OUTER_BOUND('',#377,.T.);
#280=FACE_OUTER_BOUND('',#378,.T.);
#281=FACE_OUTER_BOUND('',#379,.T.);
#282=FACE_OUTER_BOUND('',#380,.T.);
#283=FACE_OUTER_BOUND('',#381,.T.);
#284=FACE_OUTER_BOUND('',#382,.T.);
#285=FACE_OUTER_BOUND('',#383,.T.);
#286=FACE_OUTER_BOUND('',#384,.T.);
#287=FACE_OUTER_BOUND('',#385,.T.);
#288=FACE_OUTER_BOUND('',#386,.T.);
#289=FACE_OUTER_BOUND('',#388,.T.);
#290=FACE_OUTER_BOUND('',#389,.T.);
#291=FACE_OUTER_BOUND('',#390,.T.);
#292=FACE_OUTER_BOUND('',#391,.T.);
#293=FACE_OUTER_BOUND('',#392,.T.);
#294=FACE_OUTER_BOUND('',#393,.T.);
#295=FACE_OUTER_BOUND('',#394,.T.);
#296=FACE_OUTER_BOUND('',#395,.T.);
#297=FACE_OUTER_BOUND('',#396,.T.);
#298=FACE_OUTER_BOUND('',#397,.T.);
#299=FACE_OUTER_BOUND('',#398,.T.);
#300=FACE_OUTER_BOUND('',#399,.T.);
#301=FACE_OUTER_BOUND('',#400,.T.);
#302=FACE_OUTER_BOUND('',#401,.T.);
#303=FACE_OUTER_BOUND('',#402,.T.);
#304=FACE_OUTER_BOUND('',#403,.T.);
#305=FACE_OUTER_BOUND('',#404,.T.);
#306=FACE_OUTER_BOUND('',#405,.T.);
#307=FACE_OUTER_BOUND('',#406,.T.);
#308=FACE_OUTER_BOUND('',#407,.T.);
#309=FACE_OUTER_BOUND('',#408,.T.);
#310=FACE_OUTER_BOUND('',#409,.T.);
#311=FACE_OUTER_BOUND('',#411,.T.);
#312=FACE_OUTER_BOUND('',#412,.T.);
#313=FACE_OUTER_BOUND('',#413,.T.);
#314=FACE_OUTER_BOUND('',#415,.T.);
#315=FACE_OUTER_BOUND('',#416,.T.);
#316=FACE_OUTER_BOUND('',#417,.T.);
#317=FACE_OUTER_BOUND('',#418,.T.);
#318=FACE_OUTER_BOUND('',#419,.T.);
#319=FACE_OUTER_BOUND('',#421,.T.);
#320=FACE_OUTER_BOUND('',#422,.T.);
#321=FACE_OUTER_BOUND('',#423,.T.);
#322=FACE_OUTER_BOUND('',#424,.T.);
#323=FACE_OUTER_BOUND('',#425,.T.);
#324=FACE_OUTER_BOUND('',#426,.T.);
#325=FACE_OUTER_BOUND('',#428,.T.);
#326=FACE_OUTER_BOUND('',#429,.T.);
#327=FACE_OUTER_BOUND('',#430,.T.);
#328=FACE_OUTER_BOUND('',#431,.T.);
#329=FACE_OUTER_BOUND('',#432,.T.);
#330=FACE_OUTER_BOUND('',#433,.T.);
#331=FACE_OUTER_BOUND('',#434,.T.);
#332=FACE_OUTER_BOUND('',#435,.T.);
#333=FACE_OUTER_BOUND('',#436,.T.);
#334=FACE_OUTER_BOUND('',#437,.T.);
#335=FACE_OUTER_BOUND('',#438,.T.);
#336=FACE_OUTER_BOUND('',#440,.T.);
#337=FACE_OUTER_BOUND('',#441,.T.);
#338=FACE_OUTER_BOUND('',#442,.T.);
#339=FACE_OUTER_BOUND('',#443,.T.);
#340=FACE_OUTER_BOUND('',#444,.T.);
#341=FACE_OUTER_BOUND('',#446,.T.);
#342=FACE_OUTER_BOUND('',#447,.T.);
#343=FACE_OUTER_BOUND('',#448,.T.);
#344=FACE_OUTER_BOUND('',#449,.T.);
#345=FACE_OUTER_BOUND('',#450,.T.);
#346=FACE_OUTER_BOUND('',#451,.T.);
#347=FACE_OUTER_BOUND('',#452,.T.);
#348=FACE_OUTER_BOUND('',#453,.T.);
#349=FACE_OUTER_BOUND('',#454,.T.);
#350=FACE_OUTER_BOUND('',#455,.T.);
#351=FACE_OUTER_BOUND('',#456,.T.);
#352=FACE_OUTER_BOUND('',#458,.T.);
#353=FACE_OUTER_BOUND('',#460,.T.);
#354=FACE_OUTER_BOUND('',#461,.T.);
#355=FACE_OUTER_BOUND('',#462,.T.);
#356=FACE_OUTER_BOUND('',#463,.T.);
#357=FACE_OUTER_BOUND('',#464,.T.);
#358=FACE_OUTER_BOUND('',#465,.T.);
#359=FACE_OUTER_BOUND('',#466,.T.);
#360=FACE_OUTER_BOUND('',#467,.T.);
#361=FACE_OUTER_BOUND('',#468,.T.);
#362=FACE_OUTER_BOUND('',#469,.T.);
#363=FACE_OUTER_BOUND('',#470,.T.);
#364=FACE_OUTER_BOUND('',#471,.T.);
#365=FACE_OUTER_BOUND('',#472,.T.);
#366=FACE_OUTER_BOUND('',#473,.T.);
#367=FACE_OUTER_BOUND('',#474,.T.);
#368=FACE_OUTER_BOUND('',#476,.T.);
#369=EDGE_LOOP('',(#1291,#1292,#1293,#1294));
#370=EDGE_LOOP('',(#1295,#1296,#1297,#1298));
#371=EDGE_LOOP('',(#1299));
#372=EDGE_LOOP('',(#1300));
#373=EDGE_LOOP('',(#1301));
#374=EDGE_LOOP('',(#1302));
#375=EDGE_LOOP('',(#1303,#1304,#1305,#1306));
#376=EDGE_LOOP('',(#1307));
#377=EDGE_LOOP('',(#1308));
#378=EDGE_LOOP('',(#1309,#1310,#1311,#1312));
#379=EDGE_LOOP('',(#1313,#1314,#1315,#1316,#1317));
#380=EDGE_LOOP('',(#1318,#1319,#1320,#1321,#1322));
#381=EDGE_LOOP('',(#1323,#1324,#1325,#1326,#1327));
#382=EDGE_LOOP('',(#1328,#1329,#1330,#1331,#1332));
#383=EDGE_LOOP('',(#1333,#1334,#1335,#1336,#1337));
#384=EDGE_LOOP('',(#1338,#1339,#1340,#1341,#1342));
#385=EDGE_LOOP('',(#1343,#1344,#1345,#1346,#1347,#1348));
#386=EDGE_LOOP('',(#1349));
#387=EDGE_LOOP('',(#1350,#1351,#1352,#1353,#1354,#1355,#1356,#1357,#1358,
#1359,#1360,#1361,#1362,#1363,#1364,#1365,#1366,#1367,#1368,#1369,#1370));
#388=EDGE_LOOP('',(#1371,#1372,#1373,#1374,#1375));
#389=EDGE_LOOP('',(#1376,#1377,#1378,#1379,#1380,#1381,#1382,#1383,#1384,
#1385,#1386,#1387,#1388,#1389,#1390,#1391,#1392,#1393,#1394,#1395,#1396,
#1397,#1398,#1399,#1400));
#390=EDGE_LOOP('',(#1401,#1402,#1403,#1404));
#391=EDGE_LOOP('',(#1405,#1406,#1407,#1408,#1409,#1410,#1411,#1412,#1413,
#1414,#1415,#1416,#1417,#1418,#1419,#1420,#1421,#1422,#1423,#1424,#1425,
#1426,#1427,#1428,#1429,#1430));
#392=EDGE_LOOP('',(#1431,#1432,#1433,#1434,#1435));
#393=EDGE_LOOP('',(#1436));
#394=EDGE_LOOP('',(#1437,#1438,#1439,#1440));
#395=EDGE_LOOP('',(#1441,#1442,#1443,#1444,#1445,#1446));
#396=EDGE_LOOP('',(#1447,#1448,#1449,#1450));
#397=EDGE_LOOP('',(#1451,#1452,#1453,#1454));
#398=EDGE_LOOP('',(#1455,#1456,#1457,#1458,#1459,#1460,#1461,#1462,#1463,
#1464,#1465,#1466,#1467,#1468));
#399=EDGE_LOOP('',(#1469,#1470,#1471,#1472));
#400=EDGE_LOOP('',(#1473,#1474,#1475,#1476));
#401=EDGE_LOOP('',(#1477,#1478,#1479,#1480));
#402=EDGE_LOOP('',(#1481,#1482,#1483,#1484));
#403=EDGE_LOOP('',(#1485,#1486,#1487,#1488,#1489,#1490,#1491,#1492,#1493,
#1494));
#404=EDGE_LOOP('',(#1495,#1496,#1497,#1498));
#405=EDGE_LOOP('',(#1499,#1500,#1501,#1502));
#406=EDGE_LOOP('',(#1503,#1504,#1505,#1506,#1507,#1508,#1509,#1510,#1511,
#1512));
#407=EDGE_LOOP('',(#1513,#1514,#1515,#1516));
#408=EDGE_LOOP('',(#1517,#1518,#1519,#1520));
#409=EDGE_LOOP('',(#1521,#1522,#1523,#1524,#1525));
#410=EDGE_LOOP('',(#1526));
#411=EDGE_LOOP('',(#1527,#1528,#1529,#1530));
#412=EDGE_LOOP('',(#1531,#1532,#1533,#1534,#1535,#1536));
#413=EDGE_LOOP('',(#1537,#1538,#1539,#1540,#1541,#1542,#1543,#1544,#1545));
#414=EDGE_LOOP('',(#1546));
#415=EDGE_LOOP('',(#1547,#1548,#1549,#1550));
#416=EDGE_LOOP('',(#1551,#1552,#1553,#1554));
#417=EDGE_LOOP('',(#1555,#1556,#1557,#1558));
#418=EDGE_LOOP('',(#1559,#1560,#1561,#1562));
#419=EDGE_LOOP('',(#1563,#1564,#1565,#1566,#1567));
#420=EDGE_LOOP('',(#1568));
#421=EDGE_LOOP('',(#1569,#1570,#1571,#1572,#1573,#1574,#1575,#1576,#1577,
#1578,#1579,#1580));
#422=EDGE_LOOP('',(#1581,#1582,#1583,#1584,#1585,#1586));
#423=EDGE_LOOP('',(#1587,#1588,#1589,#1590));
#424=EDGE_LOOP('',(#1591,#1592,#1593,#1594));
#425=EDGE_LOOP('',(#1595,#1596,#1597,#1598));
#426=EDGE_LOOP('',(#1599,#1600,#1601,#1602,#1603,#1604,#1605,#1606,#1607));
#427=EDGE_LOOP('',(#1608));
#428=EDGE_LOOP('',(#1609,#1610,#1611,#1612));
#429=EDGE_LOOP('',(#1613,#1614,#1615,#1616,#1617));
#430=EDGE_LOOP('',(#1618,#1619,#1620,#1621,#1622));
#431=EDGE_LOOP('',(#1623,#1624,#1625,#1626,#1627,#1628));
#432=EDGE_LOOP('',(#1629,#1630,#1631,#1632,#1633));
#433=EDGE_LOOP('',(#1634,#1635,#1636,#1637,#1638));
#434=EDGE_LOOP('',(#1639,#1640,#1641,#1642,#1643));
#435=EDGE_LOOP('',(#1644,#1645,#1646,#1647,#1648));
#436=EDGE_LOOP('',(#1649,#1650,#1651,#1652,#1653,#1654));
#437=EDGE_LOOP('',(#1655,#1656,#1657,#1658,#1659,#1660));
#438=EDGE_LOOP('',(#1661));
#439=EDGE_LOOP('',(#1662,#1663,#1664,#1665,#1666,#1667,#1668,#1669,#1670,
#1671,#1672,#1673,#1674,#1675,#1676,#1677,#1678,#1679,#1680,#1681,#1682,
#1683,#1684,#1685,#1686));
#440=EDGE_LOOP('',(#1687,#1688,#1689,#1690,#1691));
#441=EDGE_LOOP('',(#1692,#1693,#1694,#1695,#1696,#1697,#1698,#1699,#1700,
#1701,#1702,#1703,#1704,#1705,#1706,#1707,#1708,#1709,#1710,#1711,#1712,
#1713,#1714,#1715,#1716,#1717,#1718,#1719,#1720,#1721,#1722));
#442=EDGE_LOOP('',(#1723,#1724,#1725,#1726));
#443=EDGE_LOOP('',(#1727,#1728,#1729,#1730,#1731,#1732,#1733,#1734,#1735,
#1736,#1737,#1738,#1739,#1740,#1741,#1742,#1743,#1744,#1745,#1746,#1747,
#1748,#1749,#1750,#1751,#1752,#1753,#1754,#1755,#1756,#1757,#1758));
#444=EDGE_LOOP('',(#1759));
#445=EDGE_LOOP('',(#1760));
#446=EDGE_LOOP('',(#1761,#1762,#1763,#1764));
#447=EDGE_LOOP('',(#1765));
#448=EDGE_LOOP('',(#1766,#1767,#1768,#1769,#1770));
#449=EDGE_LOOP('',(#1771,#1772,#1773,#1774));
#450=EDGE_LOOP('',(#1775,#1776,#1777,#1778));
#451=EDGE_LOOP('',(#1779,#1780,#1781,#1782));
#452=EDGE_LOOP('',(#1783,#1784,#1785,#1786));
#453=EDGE_LOOP('',(#1787,#1788,#1789,#1790));
#454=EDGE_LOOP('',(#1791,#1792,#1793,#1794));
#455=EDGE_LOOP('',(#1795,#1796,#1797,#1798));
#456=EDGE_LOOP('',(#1799,#1800,#1801,#1802,#1803,#1804));
#457=EDGE_LOOP('',(#1805));
#458=EDGE_LOOP('',(#1806,#1807,#1808,#1809,#1810,#1811));
#459=EDGE_LOOP('',(#1812));
#460=EDGE_LOOP('',(#1813,#1814));
#461=EDGE_LOOP('',(#1815,#1816));
#462=EDGE_LOOP('',(#1817));
#463=EDGE_LOOP('',(#1818,#1819,#1820,#1821));
#464=EDGE_LOOP('',(#1822,#1823,#1824,#1825,#1826,#1827,#1828,#1829,#1830,
#1831,#1832,#1833));
#465=EDGE_LOOP('',(#1834,#1835,#1836,#1837));
#466=EDGE_LOOP('',(#1838,#1839,#1840,#1841,#1842));
#467=EDGE_LOOP('',(#1843,#1844,#1845,#1846));
#468=EDGE_LOOP('',(#1847,#1848,#1849,#1850));
#469=EDGE_LOOP('',(#1851,#1852,#1853,#1854));
#470=EDGE_LOOP('',(#1855,#1856,#1857,#1858));
#471=EDGE_LOOP('',(#1859,#1860,#1861,#1862));
#472=EDGE_LOOP('',(#1863,#1864,#1865,#1866));
#473=EDGE_LOOP('',(#1867,#1868,#1869,#1870));
#474=EDGE_LOOP('',(#1871,#1872,#1873,#1874,#1875,#1876));
#475=EDGE_LOOP('',(#1877));
#476=EDGE_LOOP('',(#1878,#1879,#1880,#1881,#1882,#1883));
#477=EDGE_LOOP('',(#1884));
#478=LINE('',#2701,#605);
#479=LINE('',#2707,#606);
#480=LINE('',#2716,#607);
#481=LINE('',#2724,#608);
#482=LINE('',#2901,#609);
#483=LINE('',#3252,#610);
#484=LINE('',#3609,#611);
#485=LINE('',#3968,#612);
#486=LINE('',#4311,#613);
#487=LINE('',#4674,#614);
#488=LINE('',#5062,#615);
#489=LINE('',#9792,#616);
#490=LINE('',#9795,#617);
#491=LINE('',#9798,#618);
#492=LINE('',#9802,#619);
#493=LINE('',#9804,#620);
#494=LINE('',#9805,#621);
#495=LINE('',#9808,#622);
#496=LINE('',#9811,#623);
#497=LINE('',#9813,#624);
#498=LINE('',#9817,#625);
#499=LINE('',#9818,#626);
#500=LINE('',#9820,#627);
#501=LINE('',#9822,#628);
#502=LINE('',#9824,#629);
#503=LINE('',#9826,#630);
#504=LINE('',#9828,#631);
#505=LINE('',#9830,#632);
#506=LINE('',#9832,#633);
#507=LINE('',#9834,#634);
#508=LINE('',#9835,#635);
#509=LINE('',#9837,#636);
#510=LINE('',#9838,#637);
#511=LINE('',#9925,#638);
#512=LINE('',#10150,#639);
#513=LINE('',#10153,#640);
#514=LINE('',#10155,#641);
#515=LINE('',#10156,#642);
#516=LINE('',#10308,#643);
#517=LINE('',#10595,#644);
#518=LINE('',#10630,#645);
#519=LINE('',#10773,#646);
#520=LINE('',#10776,#647);
#521=LINE('',#10777,#648);
#522=LINE('',#10780,#649);
#523=LINE('',#10794,#650);
#524=LINE('',#10839,#651);
#525=LINE('',#10850,#652);
#526=LINE('',#10874,#653);
#527=LINE('',#10877,#654);
#528=LINE('',#10882,#655);
#529=LINE('',#10886,#656);
#530=LINE('',#10887,#657);
#531=LINE('',#10890,#658);
#532=LINE('',#10891,#659);
#533=LINE('',#10894,#660);
#534=LINE('',#10901,#661);
#535=LINE('',#10903,#662);
#536=LINE('',#10905,#663);
#537=LINE('',#10907,#664);
#538=LINE('',#10908,#665);
#539=LINE('',#10911,#666);
#540=LINE('',#10916,#667);
#541=LINE('',#10921,#668);
#542=LINE('',#10922,#669);
#543=LINE('',#10925,#670);
#544=LINE('',#10926,#671);
#545=LINE('',#10930,#672);
#546=LINE('',#10934,#673);
#547=LINE('',#10942,#674);
#548=LINE('',#11114,#675);
#549=LINE('',#11481,#676);
#550=LINE('',#11844,#677);
#551=LINE('',#12104,#678);
#552=LINE('',#12425,#679);
#553=LINE('',#12784,#680);
#554=LINE('',#13149,#681);
#555=LINE('',#13404,#682);
#556=LINE('',#13736,#683);
#557=LINE('',#19290,#684);
#558=LINE('',#19298,#685);
#559=LINE('',#19303,#686);
#560=LINE('',#19305,#687);
#561=LINE('',#19307,#688);
#562=LINE('',#19308,#689);
#563=LINE('',#19311,#690);
#564=LINE('',#19313,#691);
#565=LINE('',#19314,#692);
#566=LINE('',#19317,#693);
#567=LINE('',#19319,#694);
#568=LINE('',#19320,#695);
#569=LINE('',#19323,#696);
#570=LINE('',#19325,#697);
#571=LINE('',#19326,#698);
#572=LINE('',#19329,#699);
#573=LINE('',#19331,#700);
#574=LINE('',#19332,#701);
#575=LINE('',#19334,#702);
#576=LINE('',#19335,#703);
#577=LINE('',#19342,#704);
#578=LINE('',#19347,#705);
#579=LINE('',#19354,#706);
#580=LINE('',#19356,#707);
#581=LINE('',#19357,#708);
#582=LINE('',#19363,#709);
#583=LINE('',#19365,#710);
#584=LINE('',#19367,#711);
#585=LINE('',#19369,#712);
#586=LINE('',#19376,#713);
#587=LINE('',#19381,#714);
#588=LINE('',#19383,#715);
#589=LINE('',#19385,#716);
#590=LINE('',#19386,#717);
#591=LINE('',#19389,#718);
#592=LINE('',#19391,#719);
#593=LINE('',#19392,#720);
#594=LINE('',#19395,#721);
#595=LINE('',#19397,#722);
#596=LINE('',#19398,#723);
#597=LINE('',#19401,#724);
#598=LINE('',#19403,#725);
#599=LINE('',#19404,#726);
#600=LINE('',#19407,#727);
#601=LINE('',#19409,#728);
#602=LINE('',#19410,#729);
#603=LINE('',#19412,#730);
#604=LINE('',#19413,#731);
#605=VECTOR('',#2274,8.);
#606=VECTOR('',#2281,10.);
#607=VECTOR('',#2294,9.);
#608=VECTOR('',#2305,3.22275);
#609=VECTOR('',#2310,3.22275);
#610=VECTOR('',#2313,3.22275);
#611=VECTOR('',#2316,3.22275);
#612=VECTOR('',#2319,3.22275);
#613=VECTOR('',#2322,3.22275);
#614=VECTOR('',#2325,3.22275);
#615=VECTOR('',#2328,3.22275);
#616=VECTOR('',#2353,10.);
#617=VECTOR('',#2356,10.);
#618=VECTOR('',#2359,10.);
#619=VECTOR('',#2362,10.);
#620=VECTOR('',#2363,10.);
#621=VECTOR('',#2364,10.);
#622=VECTOR('',#2367,10.);
#623=VECTOR('',#2370,10.);
#624=VECTOR('',#2373,10.);
#625=VECTOR('',#2376,10.);
#626=VECTOR('',#2377,10.);
#627=VECTOR('',#2378,10.);
#628=VECTOR('',#2379,10.);
#629=VECTOR('',#2380,10.);
#630=VECTOR('',#2381,10.);
#631=VECTOR('',#2382,10.);
#632=VECTOR('',#2383,10.);
#633=VECTOR('',#2384,10.);
#634=VECTOR('',#2385,10.);
#635=VECTOR('',#2386,10.);
#636=VECTOR('',#2389,10.);
#637=VECTOR('',#2390,10.);
#638=VECTOR('',#2393,10.);
#639=VECTOR('',#2394,10.);
#640=VECTOR('',#2397,10.);
#641=VECTOR('',#2398,10.);
#642=VECTOR('',#2399,10.);
#643=VECTOR('',#2402,10.);
#644=VECTOR('',#2403,10.);
#645=VECTOR('',#2404,10.);
#646=VECTOR('',#2405,10.);
#647=VECTOR('',#2408,10.);
#648=VECTOR('',#2409,10.);
#649=VECTOR('',#2412,10.);
#650=VECTOR('',#2413,10.);
#651=VECTOR('',#2414,10.);
#652=VECTOR('',#2415,10.);
#653=VECTOR('',#2420,10.);
#654=VECTOR('',#2423,10.);
#655=VECTOR('',#2428,10.);
#656=VECTOR('',#2433,10.);
#657=VECTOR('',#2434,10.);
#658=VECTOR('',#2437,10.);
#659=VECTOR('',#2438,10.);
#660=VECTOR('',#2441,10.);
#661=VECTOR('',#2450,3.99999999999997);
#662=VECTOR('',#2453,10.);
#663=VECTOR('',#2456,10.);
#664=VECTOR('',#2459,10.);
#665=VECTOR('',#2460,10.);
#666=VECTOR('',#2463,10.);
#667=VECTOR('',#2468,10.);
#668=VECTOR('',#2473,10.);
#669=VECTOR('',#2474,10.);
#670=VECTOR('',#2477,10.);
#671=VECTOR('',#2478,10.);
#672=VECTOR('',#2483,3.99999999999997);
#673=VECTOR('',#2488,10.);
#674=VECTOR('',#2499,2.37175);
#675=VECTOR('',#2504,2.37175);
#676=VECTOR('',#2507,2.37175);
#677=VECTOR('',#2510,2.37175);
#678=VECTOR('',#2513,2.37175);
#679=VECTOR('',#2516,2.37175);
#680=VECTOR('',#2519,2.37175);
#681=VECTOR('',#2522,2.37175);
#682=VECTOR('',#2525,2.37175);
#683=VECTOR('',#2528,2.37175);
#684=VECTOR('',#2551,4.);
#685=VECTOR('',#2562,2.942);
#686=VECTOR('',#2567,10.);
#687=VECTOR('',#2568,10.);
#688=VECTOR('',#2569,10.);
#689=VECTOR('',#2570,10.);
#690=VECTOR('',#2573,10.);
#691=VECTOR('',#2574,10.);
#692=VECTOR('',#2575,10.);
#693=VECTOR('',#2578,10.);
#694=VECTOR('',#2579,10.);
#695=VECTOR('',#2580,10.);
#696=VECTOR('',#2583,10.);
#697=VECTOR('',#2584,10.);
#698=VECTOR('',#2585,10.);
#699=VECTOR('',#2588,10.);
#700=VECTOR('',#2589,10.);
#701=VECTOR('',#2590,10.);
#702=VECTOR('',#2593,10.);
#703=VECTOR('',#2594,10.);
#704=VECTOR('',#2603,10.);
#705=VECTOR('',#2608,10.);
#706=VECTOR('',#2617,10.);
#707=VECTOR('',#2618,10.);
#708=VECTOR('',#2619,10.);
#709=VECTOR('',#2626,10.);
#710=VECTOR('',#2627,10.);
#711=VECTOR('',#2630,8.);
#712=VECTOR('',#2633,10.);
#713=VECTOR('',#2642,3.933);
#714=VECTOR('',#2647,10.);
#715=VECTOR('',#2648,10.);
#716=VECTOR('',#2649,10.);
#717=VECTOR('',#2650,10.);
#718=VECTOR('',#2653,10.);
#719=VECTOR('',#2654,10.);
#720=VECTOR('',#2655,10.);
#721=VECTOR('',#2658,10.);
#722=VECTOR('',#2659,10.);
#723=VECTOR('',#2660,10.);
#724=VECTOR('',#2663,10.);
#725=VECTOR('',#2664,10.);
#726=VECTOR('',#2665,10.);
#727=VECTOR('',#2668,10.);
#728=VECTOR('',#2669,10.);
#729=VECTOR('',#2670,10.);
#730=VECTOR('',#2673,10.);
#731=VECTOR('',#2674,10.);
#732=CIRCLE('',#2118,8.);
#733=CIRCLE('',#2119,8.);
#734=CIRCLE('',#2121,10.);
#735=CIRCLE('',#2122,10.);
#736=CIRCLE('',#2127,9.);
#737=CIRCLE('',#2128,9.);
#738=CIRCLE('',#2133,3.22275);
#739=CIRCLE('',#2142,3.933);
#740=CIRCLE('',#2143,3.933);
#741=CIRCLE('',#2144,3.933);
#742=CIRCLE('',#2146,3.22275);
#743=CIRCLE('',#2152,6.5);
#744=CIRCLE('',#2153,6.5);
#745=CIRCLE('',#2155,6.5);
#746=CIRCLE('',#2157,6.5);
#747=CIRCLE('',#2169,22.);
#748=CIRCLE('',#2170,22.);
#749=CIRCLE('',#2171,3.99999999999997);
#750=CIRCLE('',#2175,22.);
#751=CIRCLE('',#2176,22.);
#752=CIRCLE('',#2177,3.99999999999997);
#753=CIRCLE('',#2183,22.);
#754=CIRCLE('',#2184,22.);
#755=CIRCLE('',#2185,3.99999999999997);
#756=CIRCLE('',#2189,3.99999999999997);
#757=CIRCLE('',#2191,22.);
#758=CIRCLE('',#2193,22.);
#759=CIRCLE('',#2197,2.37175);
#760=CIRCLE('',#2208,2.942);
#761=CIRCLE('',#2209,2.942);
#762=CIRCLE('',#2210,2.942);
#763=CIRCLE('',#2212,2.37175);
#764=CIRCLE('',#2215,4.);
#765=CIRCLE('',#2217,4.);
#766=CIRCLE('',#2222,2.942);
#767=CIRCLE('',#2223,2.942);
#768=CIRCLE('',#2234,8.);
#769=CIRCLE('',#2236,8.);
#770=CIRCLE('',#2238,8.);
#771=CIRCLE('',#2241,8.);
#772=CIRCLE('',#2242,8.);
#773=CIRCLE('',#2243,8.);
#774=CIRCLE('',#2248,3.933);
#775=CIRCLE('',#2249,3.933);
#776=VERTEX_POINT('',#2698);
#777=VERTEX_POINT('',#2700);
#778=VERTEX_POINT('',#2704);
#779=VERTEX_POINT('',#2706);
#780=VERTEX_POINT('',#2713);
#781=VERTEX_POINT('',#2715);
#782=VERTEX_POINT('',#2722);
#783=VERTEX_POINT('',#2723);
#784=VERTEX_POINT('',#2725);
#785=VERTEX_POINT('',#2838);
#786=VERTEX_POINT('',#2899);
#787=VERTEX_POINT('',#2900);
#788=VERTEX_POINT('',#2902);
#789=VERTEX_POINT('',#3250);
#790=VERTEX_POINT('',#3251);
#791=VERTEX_POINT('',#3431);
#792=VERTEX_POINT('',#3607);
#793=VERTEX_POINT('',#3608);
#794=VERTEX_POINT('',#3610);
#795=VERTEX_POINT('',#3966);
#796=VERTEX_POINT('',#3967);
#797=VERTEX_POINT('',#4137);
#798=VERTEX_POINT('',#4309);
#799=VERTEX_POINT('',#4310);
#800=VERTEX_POINT('',#4312);
#801=VERTEX_POINT('',#4672);
#802=VERTEX_POINT('',#4673);
#803=VERTEX_POINT('',#4855);
#804=VERTEX_POINT('',#5060);
#805=VERTEX_POINT('',#5061);
#806=VERTEX_POINT('',#5063);
#807=VERTEX_POINT('',#5264);
#808=VERTEX_POINT('',#5457);
#809=VERTEX_POINT('',#5459);
#810=VERTEX_POINT('',#5460);
#811=VERTEX_POINT('',#5462);
#812=VERTEX_POINT('',#5468);
#813=VERTEX_POINT('',#5686);
#814=VERTEX_POINT('',#5901);
#815=VERTEX_POINT('',#6110);
#816=VERTEX_POINT('',#6325);
#817=VERTEX_POINT('',#6540);
#818=VERTEX_POINT('',#6752);
#819=VERTEX_POINT('',#6967);
#820=VERTEX_POINT('',#7149);
#821=VERTEX_POINT('',#7151);
#822=VERTEX_POINT('',#7160);
#823=VERTEX_POINT('',#7375);
#824=VERTEX_POINT('',#7590);
#825=VERTEX_POINT('',#7802);
#826=VERTEX_POINT('',#8017);
#827=VERTEX_POINT('',#8226);
#828=VERTEX_POINT('',#8441);
#829=VERTEX_POINT('',#8656);
#830=VERTEX_POINT('',#8732);
#831=VERTEX_POINT('',#8847);
#832=VERTEX_POINT('',#8849);
#833=VERTEX_POINT('',#9685);
#834=VERTEX_POINT('',#9788);
#835=VERTEX_POINT('',#9789);
#836=VERTEX_POINT('',#9791);
#837=VERTEX_POINT('',#9793);
#838=VERTEX_POINT('',#9797);
#839=VERTEX_POINT('',#9799);
#840=VERTEX_POINT('',#9801);
#841=VERTEX_POINT('',#9803);
#842=VERTEX_POINT('',#9807);
#843=VERTEX_POINT('',#9809);
#844=VERTEX_POINT('',#9815);
#845=VERTEX_POINT('',#9816);
#846=VERTEX_POINT('',#9819);
#847=VERTEX_POINT('',#9821);
#848=VERTEX_POINT('',#9823);
#849=VERTEX_POINT('',#9825);
#850=VERTEX_POINT('',#9827);
#851=VERTEX_POINT('',#9829);
#852=VERTEX_POINT('',#9831);
#853=VERTEX_POINT('',#9833);
#854=VERTEX_POINT('',#9840);
#855=VERTEX_POINT('',#9841);
#856=VERTEX_POINT('',#9924);
#857=VERTEX_POINT('',#9926);
#858=VERTEX_POINT('',#10152);
#859=VERTEX_POINT('',#10154);
#860=VERTEX_POINT('',#10158);
#861=VERTEX_POINT('',#10307);
#862=VERTEX_POINT('',#10594);
#863=VERTEX_POINT('',#10596);
#864=VERTEX_POINT('',#10613);
#865=VERTEX_POINT('',#10629);
#866=VERTEX_POINT('',#10631);
#867=VERTEX_POINT('',#10696);
#868=VERTEX_POINT('',#10775);
#869=VERTEX_POINT('',#10779);
#870=VERTEX_POINT('',#10781);
#871=VERTEX_POINT('',#10840);
#872=VERTEX_POINT('',#10849);
#873=VERTEX_POINT('',#10851);
#874=VERTEX_POINT('',#10876);
#875=VERTEX_POINT('',#10878);
#876=VERTEX_POINT('',#10880);
#877=VERTEX_POINT('',#10883);
#878=VERTEX_POINT('',#10889);
#879=VERTEX_POINT('',#10893);
#880=VERTEX_POINT('',#10895);
#881=VERTEX_POINT('',#10898);
#882=VERTEX_POINT('',#10910);
#883=VERTEX_POINT('',#10912);
#884=VERTEX_POINT('',#10914);
#885=VERTEX_POINT('',#10917);
#886=VERTEX_POINT('',#10920);
#887=VERTEX_POINT('',#10924);
#888=VERTEX_POINT('',#10928);
#889=VERTEX_POINT('',#10932);
#890=VERTEX_POINT('',#10940);
#891=VERTEX_POINT('',#10941);
#892=VERTEX_POINT('',#10943);
#893=VERTEX_POINT('',#11047);
#894=VERTEX_POINT('',#11112);
#895=VERTEX_POINT('',#11113);
#896=VERTEX_POINT('',#11115);
#897=VERTEX_POINT('',#11479);
#898=VERTEX_POINT('',#11480);
#899=VERTEX_POINT('',#11654);
#900=VERTEX_POINT('',#11842);
#901=VERTEX_POINT('',#11843);
#902=VERTEX_POINT('',#11845);
#903=VERTEX_POINT('',#12028);
#904=VERTEX_POINT('',#12102);
#905=VERTEX_POINT('',#12103);
#906=VERTEX_POINT('',#12281);
#907=VERTEX_POINT('',#12423);
#908=VERTEX_POINT('',#12424);
#909=VERTEX_POINT('',#12426);
#910=VERTEX_POINT('',#12782);
#911=VERTEX_POINT('',#12783);
#912=VERTEX_POINT('',#12965);
#913=VERTEX_POINT('',#13147);
#914=VERTEX_POINT('',#13148);
#915=VERTEX_POINT('',#13150);
#916=VERTEX_POINT('',#13402);
#917=VERTEX_POINT('',#13403);
#918=VERTEX_POINT('',#13405);
#919=VERTEX_POINT('',#13542);
#920=VERTEX_POINT('',#13734);
#921=VERTEX_POINT('',#13735);
#922=VERTEX_POINT('',#13737);
#923=VERTEX_POINT('',#13929);
#924=VERTEX_POINT('',#14116);
#925=VERTEX_POINT('',#14118);
#926=VERTEX_POINT('',#14119);
#927=VERTEX_POINT('',#14121);
#928=VERTEX_POINT('',#14127);
#929=VERTEX_POINT('',#14336);
#930=VERTEX_POINT('',#14545);
#931=VERTEX_POINT('',#14754);
#932=VERTEX_POINT('',#14966);
#933=VERTEX_POINT('',#15175);
#934=VERTEX_POINT('',#15384);
#935=VERTEX_POINT('',#15593);
#936=VERTEX_POINT('',#15802);
#937=VERTEX_POINT('',#16011);
#938=VERTEX_POINT('',#16181);
#939=VERTEX_POINT('',#16183);
#940=VERTEX_POINT('',#16192);
#941=VERTEX_POINT('',#16401);
#942=VERTEX_POINT('',#16610);
#943=VERTEX_POINT('',#16816);
#944=VERTEX_POINT('',#17025);
#945=VERTEX_POINT('',#17234);
#946=VERTEX_POINT('',#17446);
#947=VERTEX_POINT('',#17655);
#948=VERTEX_POINT('',#17867);
#949=VERTEX_POINT('',#18076);
#950=VERTEX_POINT('',#18149);
#951=VERTEX_POINT('',#18266);
#952=VERTEX_POINT('',#18268);
#953=VERTEX_POINT('',#19188);
#954=VERTEX_POINT('',#19285);
#955=VERTEX_POINT('',#19288);
#956=VERTEX_POINT('',#19295);
#957=VERTEX_POINT('',#19297);
#958=VERTEX_POINT('',#19301);
#959=VERTEX_POINT('',#19302);
#960=VERTEX_POINT('',#19304);
#961=VERTEX_POINT('',#19306);
#962=VERTEX_POINT('',#19310);
#963=VERTEX_POINT('',#19312);
#964=VERTEX_POINT('',#19316);
#965=VERTEX_POINT('',#19318);
#966=VERTEX_POINT('',#19322);
#967=VERTEX_POINT('',#19324);
#968=VERTEX_POINT('',#19328);
#969=VERTEX_POINT('',#19330);
#970=VERTEX_POINT('',#19340);
#971=VERTEX_POINT('',#19341);
#972=VERTEX_POINT('',#19345);
#973=VERTEX_POINT('',#19346);
#974=VERTEX_POINT('',#19350);
#975=VERTEX_POINT('',#19353);
#976=VERTEX_POINT('',#19355);
#977=VERTEX_POINT('',#19359);
#978=VERTEX_POINT('',#19361);
#979=VERTEX_POINT('',#19364);
#980=VERTEX_POINT('',#19373);
#981=VERTEX_POINT('',#19375);
#982=VERTEX_POINT('',#19379);
#983=VERTEX_POINT('',#19380);
#984=VERTEX_POINT('',#19382);
#985=VERTEX_POINT('',#19384);
#986=VERTEX_POINT('',#19388);
#987=VERTEX_POINT('',#19390);
#988=VERTEX_POINT('',#19394);
#989=VERTEX_POINT('',#19396);
#990=VERTEX_POINT('',#19400);
#991=VERTEX_POINT('',#19402);
#992=VERTEX_POINT('',#19406);
#993=VERTEX_POINT('',#19408);
#994=EDGE_CURVE('',#776,#776,#732,.T.);
#995=EDGE_CURVE('',#776,#777,#478,.T.);
#996=EDGE_CURVE('',#777,#777,#733,.T.);
#997=EDGE_CURVE('',#778,#778,#734,.T.);
#998=EDGE_CURVE('',#778,#779,#479,.T.);
#999=EDGE_CURVE('',#779,#779,#735,.T.);
#1000=EDGE_CURVE('',#780,#780,#736,.T.);
#1001=EDGE_CURVE('',#780,#781,#480,.T.);
#1002=EDGE_CURVE('',#781,#781,#737,.T.);
#1003=EDGE_CURVE('',#782,#783,#481,.T.);
#1004=EDGE_CURVE('',#784,#782,#49,.T.);
#1005=EDGE_CURVE('',#785,#784,#738,.T.);
#1006=EDGE_CURVE('',#785,#783,#50,.T.);
#1007=EDGE_CURVE('',#786,#787,#482,.T.);
#1008=EDGE_CURVE('',#788,#786,#51,.F.);
#1009=EDGE_CURVE('',#782,#788,#52,.T.);
#1010=EDGE_CURVE('',#783,#787,#53,.T.);
#1011=EDGE_CURVE('',#789,#790,#483,.T.);
#1012=EDGE_CURVE('',#786,#789,#54,.F.);
#1013=EDGE_CURVE('',#787,#791,#55,.T.);
#1014=EDGE_CURVE('',#791,#790,#56,.T.);
#1015=EDGE_CURVE('',#792,#793,#484,.T.);
#1016=EDGE_CURVE('',#794,#792,#57,.F.);
#1017=EDGE_CURVE('',#789,#794,#58,.F.);
#1018=EDGE_CURVE('',#790,#793,#59,.T.);
#1019=EDGE_CURVE('',#795,#796,#485,.T.);
#1020=EDGE_CURVE('',#792,#795,#60,.F.);
#1021=EDGE_CURVE('',#793,#797,#61,.T.);
#1022=EDGE_CURVE('',#797,#796,#62,.T.);
#1023=EDGE_CURVE('',#798,#799,#486,.T.);
#1024=EDGE_CURVE('',#800,#798,#63,.F.);
#1025=EDGE_CURVE('',#795,#800,#64,.F.);
#1026=EDGE_CURVE('',#796,#799,#65,.T.);
#1027=EDGE_CURVE('',#801,#802,#487,.T.);
#1028=EDGE_CURVE('',#798,#801,#66,.F.);
#1029=EDGE_CURVE('',#799,#803,#67,.T.);
#1030=EDGE_CURVE('',#803,#802,#68,.T.);
#1031=EDGE_CURVE('',#804,#805,#488,.T.);
#1032=EDGE_CURVE('',#806,#804,#69,.T.);
#1033=EDGE_CURVE('',#801,#806,#70,.F.);
#1034=EDGE_CURVE('',#802,#807,#71,.T.);
#1035=EDGE_CURVE('',#807,#805,#72,.F.);
#1036=EDGE_CURVE('',#808,#808,#739,.F.);
#1037=EDGE_CURVE('',#809,#810,#740,.T.);
#1038=EDGE_CURVE('',#810,#811,#73,.T.);
#1039=EDGE_CURVE('',#811,#812,#74,.T.);
#1040=EDGE_CURVE('',#812,#813,#75,.T.);
#1041=EDGE_CURVE('',#813,#814,#76,.T.);
#1042=EDGE_CURVE('',#814,#815,#77,.T.);
#1043=EDGE_CURVE('',#815,#816,#78,.T.);
#1044=EDGE_CURVE('',#816,#817,#79,.T.);
#1045=EDGE_CURVE('',#817,#818,#80,.T.);
#1046=EDGE_CURVE('',#818,#819,#81,.T.);
#1047=EDGE_CURVE('',#820,#819,#741,.F.);
#1048=EDGE_CURVE('',#820,#821,#82,.T.);
#1049=EDGE_CURVE('',#821,#822,#83,.T.);
#1050=EDGE_CURVE('',#822,#823,#84,.T.);
#1051=EDGE_CURVE('',#823,#824,#85,.T.);
#1052=EDGE_CURVE('',#824,#825,#86,.T.);
#1053=EDGE_CURVE('',#825,#826,#87,.T.);
#1054=EDGE_CURVE('',#826,#827,#88,.T.);
#1055=EDGE_CURVE('',#827,#828,#89,.T.);
#1056=EDGE_CURVE('',#828,#829,#90,.T.);
#1057=EDGE_CURVE('',#829,#809,#91,.T.);
#1058=EDGE_CURVE('',#805,#830,#92,.F.);
#1059=EDGE_CURVE('',#831,#830,#742,.T.);
#1060=EDGE_CURVE('',#832,#831,#93,.T.);
#1061=EDGE_CURVE('',#804,#832,#94,.T.);
#1062=EDGE_CURVE('',#819,#831,#95,.T.);
#1063=EDGE_CURVE('',#784,#810,#96,.T.);
#1064=EDGE_CURVE('',#809,#785,#97,.T.);
#1065=EDGE_CURVE('',#833,#820,#98,.T.);
#1066=EDGE_CURVE('',#830,#833,#99,.T.);
#1067=EDGE_CURVE('',#834,#835,#743,.T.);
#1068=EDGE_CURVE('',#835,#836,#489,.T.);
#1069=EDGE_CURVE('',#836,#837,#744,.T.);
#1070=EDGE_CURVE('',#837,#834,#490,.T.);
#1071=EDGE_CURVE('',#834,#838,#491,.T.);
#1072=EDGE_CURVE('',#839,#838,#745,.T.);
#1073=EDGE_CURVE('',#839,#840,#492,.T.);
#1074=EDGE_CURVE('',#841,#840,#493,.T.);
#1075=EDGE_CURVE('',#835,#841,#494,.T.);
#1076=EDGE_CURVE('',#838,#842,#495,.T.);
#1077=EDGE_CURVE('',#842,#843,#746,.T.);
#1078=EDGE_CURVE('',#843,#839,#496,.T.);
#1079=EDGE_CURVE('',#837,#842,#497,.T.);
#1080=EDGE_CURVE('',#844,#845,#498,.T.);
#1081=EDGE_CURVE('',#845,#843,#499,.T.);
#1082=EDGE_CURVE('',#846,#836,#500,.T.);
#1083=EDGE_CURVE('',#846,#847,#501,.T.);
#1084=EDGE_CURVE('',#848,#847,#502,.T.);
#1085=EDGE_CURVE('',#848,#849,#503,.T.);
#1086=EDGE_CURVE('',#850,#849,#504,.T.);
#1087=EDGE_CURVE('',#851,#850,#505,.T.);
#1088=EDGE_CURVE('',#851,#852,#506,.T.);
#1089=EDGE_CURVE('',#852,#853,#507,.T.);
#1090=EDGE_CURVE('',#844,#853,#508,.T.);
#1091=EDGE_CURVE('',#841,#850,#509,.T.);
#1092=EDGE_CURVE('',#840,#851,#510,.T.);
#1093=EDGE_CURVE('',#854,#855,#100,.T.);
#1094=EDGE_CURVE('',#854,#856,#511,.T.);
#1095=EDGE_CURVE('',#857,#856,#101,.T.);
#1096=EDGE_CURVE('',#855,#857,#512,.T.);
#1097=EDGE_CURVE('',#858,#854,#513,.T.);
#1098=EDGE_CURVE('',#858,#859,#514,.T.);
#1099=EDGE_CURVE('',#856,#859,#515,.T.);
#1100=EDGE_CURVE('',#860,#858,#102,.T.);
#1101=EDGE_CURVE('',#861,#860,#516,.T.);
#1102=EDGE_CURVE('',#859,#861,#103,.T.);
#1103=EDGE_CURVE('',#855,#862,#517,.T.);
#1104=EDGE_CURVE('',#863,#862,#104,.T.);
#1105=EDGE_CURVE('',#864,#863,#105,.T.);
#1106=EDGE_CURVE('',#865,#864,#518,.T.);
#1107=EDGE_CURVE('',#866,#865,#106,.T.);
#1108=EDGE_CURVE('',#866,#867,#107,.T.);
#1109=EDGE_CURVE('',#867,#860,#519,.T.);
#1110=EDGE_CURVE('',#857,#868,#520,.T.);
#1111=EDGE_CURVE('',#862,#868,#521,.T.);
#1112=EDGE_CURVE('',#866,#869,#522,.T.);
#1113=EDGE_CURVE('',#870,#869,#108,.T.);
#1114=EDGE_CURVE('',#867,#870,#523,.T.);
#1115=EDGE_CURVE('',#870,#861,#524,.T.);
#1116=EDGE_CURVE('',#871,#869,#109,.T.);
#1117=EDGE_CURVE('',#871,#872,#525,.T.);
#1118=EDGE_CURVE('',#873,#872,#110,.T.);
#1119=EDGE_CURVE('',#868,#873,#111,.T.);
#1120=EDGE_CURVE('',#873,#863,#526,.T.);
#1121=EDGE_CURVE('',#872,#874,#527,.T.);
#1122=EDGE_CURVE('',#875,#874,#747,.T.);
#1123=EDGE_CURVE('',#876,#875,#748,.T.);
#1124=EDGE_CURVE('',#876,#873,#528,.T.);
#1125=EDGE_CURVE('',#877,#877,#749,.T.);
#1126=EDGE_CURVE('',#863,#844,#529,.T.);
#1127=EDGE_CURVE('',#853,#864,#530,.T.);
#1128=EDGE_CURVE('',#878,#876,#531,.T.);
#1129=EDGE_CURVE('',#845,#878,#532,.T.);
#1130=EDGE_CURVE('',#879,#852,#533,.T.);
#1131=EDGE_CURVE('',#878,#880,#750,.T.);
#1132=EDGE_CURVE('',#880,#879,#751,.T.);
#1133=EDGE_CURVE('',#881,#881,#752,.T.);
#1134=EDGE_CURVE('',#877,#881,#534,.T.);
#1135=EDGE_CURVE('',#875,#880,#535,.T.);
#1136=EDGE_CURVE('',#874,#879,#536,.T.);
#1137=EDGE_CURVE('',#865,#848,#537,.T.);
#1138=EDGE_CURVE('',#847,#866,#538,.T.);
#1139=EDGE_CURVE('',#869,#882,#539,.T.);
#1140=EDGE_CURVE('',#882,#883,#753,.T.);
#1141=EDGE_CURVE('',#883,#884,#754,.T.);
#1142=EDGE_CURVE('',#884,#871,#540,.T.);
#1143=EDGE_CURVE('',#885,#885,#755,.T.);
#1144=EDGE_CURVE('',#886,#884,#541,.T.);
#1145=EDGE_CURVE('',#849,#886,#542,.T.);
#1146=EDGE_CURVE('',#887,#846,#543,.T.);
#1147=EDGE_CURVE('',#882,#887,#544,.T.);
#1148=EDGE_CURVE('',#888,#888,#756,.T.);
#1149=EDGE_CURVE('',#888,#885,#545,.T.);
#1150=EDGE_CURVE('',#887,#889,#757,.T.);
#1151=EDGE_CURVE('',#889,#883,#546,.T.);
#1152=EDGE_CURVE('',#889,#886,#758,.T.);
#1153=EDGE_CURVE('',#890,#891,#547,.T.);
#1154=EDGE_CURVE('',#892,#890,#112,.T.);
#1155=EDGE_CURVE('',#893,#892,#759,.T.);
#1156=EDGE_CURVE('',#893,#891,#113,.T.);
#1157=EDGE_CURVE('',#894,#895,#548,.T.);
#1158=EDGE_CURVE('',#896,#894,#114,.F.);
#1159=EDGE_CURVE('',#890,#896,#115,.T.);
#1160=EDGE_CURVE('',#891,#895,#116,.T.);
#1161=EDGE_CURVE('',#897,#898,#549,.T.);
#1162=EDGE_CURVE('',#894,#897,#117,.F.);
#1163=EDGE_CURVE('',#895,#899,#118,.T.);
#1164=EDGE_CURVE('',#899,#898,#119,.T.);
#1165=EDGE_CURVE('',#900,#901,#550,.T.);
#1166=EDGE_CURVE('',#902,#900,#120,.F.);
#1167=EDGE_CURVE('',#897,#902,#121,.F.);
#1168=EDGE_CURVE('',#898,#903,#122,.T.);
#1169=EDGE_CURVE('',#903,#901,#123,.T.);
#1170=EDGE_CURVE('',#904,#905,#551,.T.);
#1171=EDGE_CURVE('',#900,#904,#124,.F.);
#1172=EDGE_CURVE('',#901,#906,#125,.T.);
#1173=EDGE_CURVE('',#906,#905,#126,.T.);
#1174=EDGE_CURVE('',#907,#908,#552,.T.);
#1175=EDGE_CURVE('',#909,#907,#127,.F.);
#1176=EDGE_CURVE('',#904,#909,#128,.F.);
#1177=EDGE_CURVE('',#905,#908,#129,.T.);
#1178=EDGE_CURVE('',#910,#911,#553,.T.);
#1179=EDGE_CURVE('',#907,#910,#130,.F.);
#1180=EDGE_CURVE('',#908,#912,#131,.T.);
#1181=EDGE_CURVE('',#912,#911,#132,.T.);
#1182=EDGE_CURVE('',#913,#914,#554,.T.);
#1183=EDGE_CURVE('',#915,#913,#133,.T.);
#1184=EDGE_CURVE('',#910,#915,#134,.F.);
#1185=EDGE_CURVE('',#911,#914,#135,.T.);
#1186=EDGE_CURVE('',#916,#917,#555,.T.);
#1187=EDGE_CURVE('',#918,#916,#136,.T.);
#1188=EDGE_CURVE('',#913,#918,#137,.T.);
#1189=EDGE_CURVE('',#914,#919,#138,.T.);
#1190=EDGE_CURVE('',#919,#917,#139,.T.);
#1191=EDGE_CURVE('',#920,#921,#556,.T.);
#1192=EDGE_CURVE('',#922,#920,#140,.T.);
#1193=EDGE_CURVE('',#916,#922,#141,.T.);
#1194=EDGE_CURVE('',#917,#923,#142,.T.);
#1195=EDGE_CURVE('',#923,#921,#143,.F.);
#1196=EDGE_CURVE('',#924,#924,#760,.F.);
#1197=EDGE_CURVE('',#925,#926,#761,.T.);
#1198=EDGE_CURVE('',#926,#927,#144,.T.);
#1199=EDGE_CURVE('',#927,#928,#145,.T.);
#1200=EDGE_CURVE('',#928,#929,#146,.T.);
#1201=EDGE_CURVE('',#929,#930,#147,.T.);
#1202=EDGE_CURVE('',#930,#931,#148,.T.);
#1203=EDGE_CURVE('',#931,#932,#149,.T.);
#1204=EDGE_CURVE('',#932,#933,#150,.T.);
#1205=EDGE_CURVE('',#933,#934,#151,.T.);
#1206=EDGE_CURVE('',#934,#935,#152,.T.);
#1207=EDGE_CURVE('',#935,#936,#153,.T.);
#1208=EDGE_CURVE('',#936,#937,#154,.T.);
#1209=EDGE_CURVE('',#938,#937,#762,.T.);
#1210=EDGE_CURVE('',#938,#939,#155,.T.);
#1211=EDGE_CURVE('',#939,#940,#156,.T.);
#1212=EDGE_CURVE('',#940,#941,#157,.T.);
#1213=EDGE_CURVE('',#941,#942,#158,.T.);
#1214=EDGE_CURVE('',#942,#943,#159,.T.);
#1215=EDGE_CURVE('',#943,#944,#160,.T.);
#1216=EDGE_CURVE('',#944,#945,#161,.T.);
#1217=EDGE_CURVE('',#945,#946,#162,.T.);
#1218=EDGE_CURVE('',#946,#947,#163,.T.);
#1219=EDGE_CURVE('',#947,#948,#164,.T.);
#1220=EDGE_CURVE('',#948,#949,#165,.T.);
#1221=EDGE_CURVE('',#949,#925,#166,.T.);
#1222=EDGE_CURVE('',#921,#950,#167,.F.);
#1223=EDGE_CURVE('',#951,#950,#763,.T.);
#1224=EDGE_CURVE('',#952,#951,#168,.T.);
#1225=EDGE_CURVE('',#920,#952,#169,.T.);
#1226=EDGE_CURVE('',#937,#951,#170,.T.);
#1227=EDGE_CURVE('',#892,#926,#171,.T.);
#1228=EDGE_CURVE('',#925,#893,#172,.T.);
#1229=EDGE_CURVE('',#953,#938,#173,.T.);
#1230=EDGE_CURVE('',#950,#953,#174,.T.);
#1231=EDGE_CURVE('',#954,#954,#764,.T.);
#1232=EDGE_CURVE('',#955,#955,#765,.T.);
#1233=EDGE_CURVE('',#955,#954,#557,.T.);
#1234=EDGE_CURVE('',#956,#956,#766,.T.);
#1235=EDGE_CURVE('',#956,#957,#558,.T.);
#1236=EDGE_CURVE('',#957,#957,#767,.T.);
#1237=EDGE_CURVE('',#958,#959,#559,.T.);
#1238=EDGE_CURVE('',#959,#960,#560,.T.);
#1239=EDGE_CURVE('',#961,#960,#561,.T.);
#1240=EDGE_CURVE('',#958,#961,#562,.T.);
#1241=EDGE_CURVE('',#962,#958,#563,.T.);
#1242=EDGE_CURVE('',#963,#961,#564,.T.);
#1243=EDGE_CURVE('',#962,#963,#565,.T.);
#1244=EDGE_CURVE('',#964,#962,#566,.T.);
#1245=EDGE_CURVE('',#965,#963,#567,.T.);
#1246=EDGE_CURVE('',#964,#965,#568,.T.);
#1247=EDGE_CURVE('',#966,#964,#569,.T.);
#1248=EDGE_CURVE('',#967,#965,#570,.T.);
#1249=EDGE_CURVE('',#966,#967,#571,.T.);
#1250=EDGE_CURVE('',#968,#966,#572,.T.);
#1251=EDGE_CURVE('',#969,#967,#573,.T.);
#1252=EDGE_CURVE('',#968,#969,#574,.T.);
#1253=EDGE_CURVE('',#959,#968,#575,.T.);
#1254=EDGE_CURVE('',#960,#969,#576,.T.);
#1255=EDGE_CURVE('',#970,#971,#577,.T.);
#1256=EDGE_CURVE('',#971,#970,#768,.T.);
#1257=EDGE_CURVE('',#972,#973,#578,.T.);
#1258=EDGE_CURVE('',#973,#972,#769,.T.);
#1259=EDGE_CURVE('',#974,#974,#770,.T.);
#1260=EDGE_CURVE('',#970,#975,#579,.T.);
#1261=EDGE_CURVE('',#976,#975,#580,.T.);
#1262=EDGE_CURVE('',#971,#976,#581,.T.);
#1263=EDGE_CURVE('',#975,#977,#771,.T.);
#1264=EDGE_CURVE('',#978,#976,#772,.T.);
#1265=EDGE_CURVE('',#972,#978,#582,.T.);
#1266=EDGE_CURVE('',#973,#979,#583,.T.);
#1267=EDGE_CURVE('',#977,#979,#773,.T.);
#1268=EDGE_CURVE('',#977,#974,#584,.T.);
#1269=EDGE_CURVE('',#979,#978,#585,.T.);
#1270=EDGE_CURVE('',#980,#980,#774,.T.);
#1271=EDGE_CURVE('',#980,#981,#586,.T.);
#1272=EDGE_CURVE('',#981,#981,#775,.T.);
#1273=EDGE_CURVE('',#982,#983,#587,.T.);
#1274=EDGE_CURVE('',#983,#984,#588,.T.);
#1275=EDGE_CURVE('',#985,#984,#589,.T.);
#1276=EDGE_CURVE('',#982,#985,#590,.T.);
#1277=EDGE_CURVE('',#986,#982,#591,.T.);
#1278=EDGE_CURVE('',#987,#985,#592,.T.);
#1279=EDGE_CURVE('',#986,#987,#593,.T.);
#1280=EDGE_CURVE('',#988,#986,#594,.T.);
#1281=EDGE_CURVE('',#989,#987,#595,.T.);
#1282=EDGE_CURVE('',#988,#989,#596,.T.);
#1283=EDGE_CURVE('',#990,#988,#597,.T.);
#1284=EDGE_CURVE('',#991,#989,#598,.T.);
#1285=EDGE_CURVE('',#990,#991,#599,.T.);
#1286=EDGE_CURVE('',#992,#990,#600,.T.);
#1287=EDGE_CURVE('',#993,#991,#601,.T.);
#1288=EDGE_CURVE('',#992,#993,#602,.T.);
#1289=EDGE_CURVE('',#983,#992,#603,.T.);
#1290=EDGE_CURVE('',#984,#993,#604,.T.);
#1291=ORIENTED_EDGE('',*,*,#994,.T.);
#1292=ORIENTED_EDGE('',*,*,#995,.T.);
#1293=ORIENTED_EDGE('',*,*,#996,.F.);
#1294=ORIENTED_EDGE('',*,*,#995,.F.);
#1295=ORIENTED_EDGE('',*,*,#997,.F.);
#1296=ORIENTED_EDGE('',*,*,#998,.T.);
#1297=ORIENTED_EDGE('',*,*,#999,.T.);
#1298=ORIENTED_EDGE('',*,*,#998,.F.);
#1299=ORIENTED_EDGE('',*,*,#997,.T.);
#1300=ORIENTED_EDGE('',*,*,#996,.T.);
#1301=ORIENTED_EDGE('',*,*,#999,.F.);
#1302=ORIENTED_EDGE('',*,*,#994,.F.);
#1303=ORIENTED_EDGE('',*,*,#1000,.F.);
#1304=ORIENTED_EDGE('',*,*,#1001,.T.);
#1305=ORIENTED_EDGE('',*,*,#1002,.T.);
#1306=ORIENTED_EDGE('',*,*,#1001,.F.);
#1307=ORIENTED_EDGE('',*,*,#1000,.T.);
#1308=ORIENTED_EDGE('',*,*,#1002,.F.);
#1309=ORIENTED_EDGE('',*,*,#1003,.F.);
#1310=ORIENTED_EDGE('',*,*,#1004,.F.);
#1311=ORIENTED_EDGE('',*,*,#1005,.F.);
#1312=ORIENTED_EDGE('',*,*,#1006,.T.);
#1313=ORIENTED_EDGE('',*,*,#1007,.F.);
#1314=ORIENTED_EDGE('',*,*,#1008,.F.);
#1315=ORIENTED_EDGE('',*,*,#1009,.F.);
#1316=ORIENTED_EDGE('',*,*,#1003,.T.);
#1317=ORIENTED_EDGE('',*,*,#1010,.T.);
#1318=ORIENTED_EDGE('',*,*,#1011,.F.);
#1319=ORIENTED_EDGE('',*,*,#1012,.F.);
#1320=ORIENTED_EDGE('',*,*,#1007,.T.);
#1321=ORIENTED_EDGE('',*,*,#1013,.T.);
#1322=ORIENTED_EDGE('',*,*,#1014,.T.);
#1323=ORIENTED_EDGE('',*,*,#1015,.F.);
#1324=ORIENTED_EDGE('',*,*,#1016,.F.);
#1325=ORIENTED_EDGE('',*,*,#1017,.F.);
#1326=ORIENTED_EDGE('',*,*,#1011,.T.);
#1327=ORIENTED_EDGE('',*,*,#1018,.T.);
#1328=ORIENTED_EDGE('',*,*,#1019,.F.);
#1329=ORIENTED_EDGE('',*,*,#1020,.F.);
#1330=ORIENTED_EDGE('',*,*,#1015,.T.);
#1331=ORIENTED_EDGE('',*,*,#1021,.T.);
#1332=ORIENTED_EDGE('',*,*,#1022,.T.);
#1333=ORIENTED_EDGE('',*,*,#1023,.F.);
#1334=ORIENTED_EDGE('',*,*,#1024,.F.);
#1335=ORIENTED_EDGE('',*,*,#1025,.F.);
#1336=ORIENTED_EDGE('',*,*,#1019,.T.);
#1337=ORIENTED_EDGE('',*,*,#1026,.T.);
#1338=ORIENTED_EDGE('',*,*,#1027,.F.);
#1339=ORIENTED_EDGE('',*,*,#1028,.F.);
#1340=ORIENTED_EDGE('',*,*,#1023,.T.);
#1341=ORIENTED_EDGE('',*,*,#1029,.T.);
#1342=ORIENTED_EDGE('',*,*,#1030,.T.);
#1343=ORIENTED_EDGE('',*,*,#1031,.F.);
#1344=ORIENTED_EDGE('',*,*,#1032,.F.);
#1345=ORIENTED_EDGE('',*,*,#1033,.F.);
#1346=ORIENTED_EDGE('',*,*,#1027,.T.);
#1347=ORIENTED_EDGE('',*,*,#1034,.T.);
#1348=ORIENTED_EDGE('',*,*,#1035,.T.);
#1349=ORIENTED_EDGE('',*,*,#1036,.T.);
#1350=ORIENTED_EDGE('',*,*,#1037,.T.);
#1351=ORIENTED_EDGE('',*,*,#1038,.T.);
#1352=ORIENTED_EDGE('',*,*,#1039,.T.);
#1353=ORIENTED_EDGE('',*,*,#1040,.T.);
#1354=ORIENTED_EDGE('',*,*,#1041,.T.);
#1355=ORIENTED_EDGE('',*,*,#1042,.T.);
#1356=ORIENTED_EDGE('',*,*,#1043,.T.);
#1357=ORIENTED_EDGE('',*,*,#1044,.T.);
#1358=ORIENTED_EDGE('',*,*,#1045,.T.);
#1359=ORIENTED_EDGE('',*,*,#1046,.T.);
#1360=ORIENTED_EDGE('',*,*,#1047,.F.);
#1361=ORIENTED_EDGE('',*,*,#1048,.T.);
#1362=ORIENTED_EDGE('',*,*,#1049,.T.);
#1363=ORIENTED_EDGE('',*,*,#1050,.T.);
#1364=ORIENTED_EDGE('',*,*,#1051,.T.);
#1365=ORIENTED_EDGE('',*,*,#1052,.T.);
#1366=ORIENTED_EDGE('',*,*,#1053,.T.);
#1367=ORIENTED_EDGE('',*,*,#1054,.T.);
#1368=ORIENTED_EDGE('',*,*,#1055,.T.);
#1369=ORIENTED_EDGE('',*,*,#1056,.T.);
#1370=ORIENTED_EDGE('',*,*,#1057,.T.);
#1371=ORIENTED_EDGE('',*,*,#1031,.T.);
#1372=ORIENTED_EDGE('',*,*,#1058,.T.);
#1373=ORIENTED_EDGE('',*,*,#1059,.F.);
#1374=ORIENTED_EDGE('',*,*,#1060,.F.);
#1375=ORIENTED_EDGE('',*,*,#1061,.F.);
#1376=ORIENTED_EDGE('',*,*,#1062,.F.);
#1377=ORIENTED_EDGE('',*,*,#1046,.F.);
#1378=ORIENTED_EDGE('',*,*,#1045,.F.);
#1379=ORIENTED_EDGE('',*,*,#1044,.F.);
#1380=ORIENTED_EDGE('',*,*,#1043,.F.);
#1381=ORIENTED_EDGE('',*,*,#1042,.F.);
#1382=ORIENTED_EDGE('',*,*,#1041,.F.);
#1383=ORIENTED_EDGE('',*,*,#1040,.F.);
#1384=ORIENTED_EDGE('',*,*,#1039,.F.);
#1385=ORIENTED_EDGE('',*,*,#1038,.F.);
#1386=ORIENTED_EDGE('',*,*,#1063,.F.);
#1387=ORIENTED_EDGE('',*,*,#1004,.T.);
#1388=ORIENTED_EDGE('',*,*,#1009,.T.);
#1389=ORIENTED_EDGE('',*,*,#1008,.T.);
#1390=ORIENTED_EDGE('',*,*,#1012,.T.);
#1391=ORIENTED_EDGE('',*,*,#1017,.T.);
#1392=ORIENTED_EDGE('',*,*,#1016,.T.);
#1393=ORIENTED_EDGE('',*,*,#1020,.T.);
#1394=ORIENTED_EDGE('',*,*,#1025,.T.);
#1395=ORIENTED_EDGE('',*,*,#1024,.T.);
#1396=ORIENTED_EDGE('',*,*,#1028,.T.);
#1397=ORIENTED_EDGE('',*,*,#1033,.T.);
#1398=ORIENTED_EDGE('',*,*,#1032,.T.);
#1399=ORIENTED_EDGE('',*,*,#1061,.T.);
#1400=ORIENTED_EDGE('',*,*,#1060,.T.);
#1401=ORIENTED_EDGE('',*,*,#1037,.F.);
#1402=ORIENTED_EDGE('',*,*,#1064,.T.);
#1403=ORIENTED_EDGE('',*,*,#1005,.T.);
#1404=ORIENTED_EDGE('',*,*,#1063,.T.);
#1405=ORIENTED_EDGE('',*,*,#1065,.F.);
#1406=ORIENTED_EDGE('',*,*,#1066,.F.);
#1407=ORIENTED_EDGE('',*,*,#1058,.F.);
#1408=ORIENTED_EDGE('',*,*,#1035,.F.);
#1409=ORIENTED_EDGE('',*,*,#1034,.F.);
#1410=ORIENTED_EDGE('',*,*,#1030,.F.);
#1411=ORIENTED_EDGE('',*,*,#1029,.F.);
#1412=ORIENTED_EDGE('',*,*,#1026,.F.);
#1413=ORIENTED_EDGE('',*,*,#1022,.F.);
#1414=ORIENTED_EDGE('',*,*,#1021,.F.);
#1415=ORIENTED_EDGE('',*,*,#1018,.F.);
#1416=ORIENTED_EDGE('',*,*,#1014,.F.);
#1417=ORIENTED_EDGE('',*,*,#1013,.F.);
#1418=ORIENTED_EDGE('',*,*,#1010,.F.);
#1419=ORIENTED_EDGE('',*,*,#1006,.F.);
#1420=ORIENTED_EDGE('',*,*,#1064,.F.);
#1421=ORIENTED_EDGE('',*,*,#1057,.F.);
#1422=ORIENTED_EDGE('',*,*,#1056,.F.);
#1423=ORIENTED_EDGE('',*,*,#1055,.F.);
#1424=ORIENTED_EDGE('',*,*,#1054,.F.);
#1425=ORIENTED_EDGE('',*,*,#1053,.F.);
#1426=ORIENTED_EDGE('',*,*,#1052,.F.);
#1427=ORIENTED_EDGE('',*,*,#1051,.F.);
#1428=ORIENTED_EDGE('',*,*,#1050,.F.);
#1429=ORIENTED_EDGE('',*,*,#1049,.F.);
#1430=ORIENTED_EDGE('',*,*,#1048,.F.);
#1431=ORIENTED_EDGE('',*,*,#1065,.T.);
#1432=ORIENTED_EDGE('',*,*,#1047,.T.);
#1433=ORIENTED_EDGE('',*,*,#1062,.T.);
#1434=ORIENTED_EDGE('',*,*,#1059,.T.);
#1435=ORIENTED_EDGE('',*,*,#1066,.T.);
#1436=ORIENTED_EDGE('',*,*,#1036,.F.);
#1437=ORIENTED_EDGE('',*,*,#1067,.T.);
#1438=ORIENTED_EDGE('',*,*,#1068,.T.);
#1439=ORIENTED_EDGE('',*,*,#1069,.T.);
#1440=ORIENTED_EDGE('',*,*,#1070,.T.);
#1441=ORIENTED_EDGE('',*,*,#1067,.F.);
#1442=ORIENTED_EDGE('',*,*,#1071,.T.);
#1443=ORIENTED_EDGE('',*,*,#1072,.F.);
#1444=ORIENTED_EDGE('',*,*,#1073,.T.);
#1445=ORIENTED_EDGE('',*,*,#1074,.F.);
#1446=ORIENTED_EDGE('',*,*,#1075,.F.);
#1447=ORIENTED_EDGE('',*,*,#1072,.T.);
#1448=ORIENTED_EDGE('',*,*,#1076,.T.);
#1449=ORIENTED_EDGE('',*,*,#1077,.T.);
#1450=ORIENTED_EDGE('',*,*,#1078,.T.);
#1451=ORIENTED_EDGE('',*,*,#1070,.F.);
#1452=ORIENTED_EDGE('',*,*,#1079,.T.);
#1453=ORIENTED_EDGE('',*,*,#1076,.F.);
#1454=ORIENTED_EDGE('',*,*,#1071,.F.);
#1455=ORIENTED_EDGE('',*,*,#1080,.T.);
#1456=ORIENTED_EDGE('',*,*,#1081,.T.);
#1457=ORIENTED_EDGE('',*,*,#1077,.F.);
#1458=ORIENTED_EDGE('',*,*,#1079,.F.);
#1459=ORIENTED_EDGE('',*,*,#1069,.F.);
#1460=ORIENTED_EDGE('',*,*,#1082,.F.);
#1461=ORIENTED_EDGE('',*,*,#1083,.T.);
#1462=ORIENTED_EDGE('',*,*,#1084,.F.);
#1463=ORIENTED_EDGE('',*,*,#1085,.T.);
#1464=ORIENTED_EDGE('',*,*,#1086,.F.);
#1465=ORIENTED_EDGE('',*,*,#1087,.F.);
#1466=ORIENTED_EDGE('',*,*,#1088,.T.);
#1467=ORIENTED_EDGE('',*,*,#1089,.T.);
#1468=ORIENTED_EDGE('',*,*,#1090,.F.);
#1469=ORIENTED_EDGE('',*,*,#1087,.T.);
#1470=ORIENTED_EDGE('',*,*,#1091,.F.);
#1471=ORIENTED_EDGE('',*,*,#1074,.T.);
#1472=ORIENTED_EDGE('',*,*,#1092,.T.);
#1473=ORIENTED_EDGE('',*,*,#1093,.F.);
#1474=ORIENTED_EDGE('',*,*,#1094,.T.);
#1475=ORIENTED_EDGE('',*,*,#1095,.F.);
#1476=ORIENTED_EDGE('',*,*,#1096,.F.);
#1477=ORIENTED_EDGE('',*,*,#1097,.F.);
#1478=ORIENTED_EDGE('',*,*,#1098,.T.);
#1479=ORIENTED_EDGE('',*,*,#1099,.F.);
#1480=ORIENTED_EDGE('',*,*,#1094,.F.);
#1481=ORIENTED_EDGE('',*,*,#1100,.F.);
#1482=ORIENTED_EDGE('',*,*,#1101,.F.);
#1483=ORIENTED_EDGE('',*,*,#1102,.F.);
#1484=ORIENTED_EDGE('',*,*,#1098,.F.);
#1485=ORIENTED_EDGE('',*,*,#1100,.T.);
#1486=ORIENTED_EDGE('',*,*,#1097,.T.);
#1487=ORIENTED_EDGE('',*,*,#1093,.T.);
#1488=ORIENTED_EDGE('',*,*,#1103,.T.);
#1489=ORIENTED_EDGE('',*,*,#1104,.F.);
#1490=ORIENTED_EDGE('',*,*,#1105,.F.);
#1491=ORIENTED_EDGE('',*,*,#1106,.F.);
#1492=ORIENTED_EDGE('',*,*,#1107,.F.);
#1493=ORIENTED_EDGE('',*,*,#1108,.T.);
#1494=ORIENTED_EDGE('',*,*,#1109,.T.);
#1495=ORIENTED_EDGE('',*,*,#1096,.T.);
#1496=ORIENTED_EDGE('',*,*,#1110,.T.);
#1497=ORIENTED_EDGE('',*,*,#1111,.F.);
#1498=ORIENTED_EDGE('',*,*,#1103,.F.);
#1499=ORIENTED_EDGE('',*,*,#1112,.T.);
#1500=ORIENTED_EDGE('',*,*,#1113,.F.);
#1501=ORIENTED_EDGE('',*,*,#1114,.F.);
#1502=ORIENTED_EDGE('',*,*,#1108,.F.);
#1503=ORIENTED_EDGE('',*,*,#1102,.T.);
#1504=ORIENTED_EDGE('',*,*,#1115,.F.);
#1505=ORIENTED_EDGE('',*,*,#1113,.T.);
#1506=ORIENTED_EDGE('',*,*,#1116,.F.);
#1507=ORIENTED_EDGE('',*,*,#1117,.T.);
#1508=ORIENTED_EDGE('',*,*,#1118,.F.);
#1509=ORIENTED_EDGE('',*,*,#1119,.F.);
#1510=ORIENTED_EDGE('',*,*,#1110,.F.);
#1511=ORIENTED_EDGE('',*,*,#1095,.T.);
#1512=ORIENTED_EDGE('',*,*,#1099,.T.);
#1513=ORIENTED_EDGE('',*,*,#1101,.T.);
#1514=ORIENTED_EDGE('',*,*,#1109,.F.);
#1515=ORIENTED_EDGE('',*,*,#1114,.T.);
#1516=ORIENTED_EDGE('',*,*,#1115,.T.);
#1517=ORIENTED_EDGE('',*,*,#1120,.T.);
#1518=ORIENTED_EDGE('',*,*,#1104,.T.);
#1519=ORIENTED_EDGE('',*,*,#1111,.T.);
#1520=ORIENTED_EDGE('',*,*,#1119,.T.);
#1521=ORIENTED_EDGE('',*,*,#1118,.T.);
#1522=ORIENTED_EDGE('',*,*,#1121,.T.);
#1523=ORIENTED_EDGE('',*,*,#1122,.F.);
#1524=ORIENTED_EDGE('',*,*,#1123,.F.);
#1525=ORIENTED_EDGE('',*,*,#1124,.T.);
#1526=ORIENTED_EDGE('',*,*,#1125,.F.);
#1527=ORIENTED_EDGE('',*,*,#1105,.T.);
#1528=ORIENTED_EDGE('',*,*,#1126,.T.);
#1529=ORIENTED_EDGE('',*,*,#1090,.T.);
#1530=ORIENTED_EDGE('',*,*,#1127,.T.);
#1531=ORIENTED_EDGE('',*,*,#1124,.F.);
#1532=ORIENTED_EDGE('',*,*,#1128,.F.);
#1533=ORIENTED_EDGE('',*,*,#1129,.F.);
#1534=ORIENTED_EDGE('',*,*,#1080,.F.);
#1535=ORIENTED_EDGE('',*,*,#1126,.F.);
#1536=ORIENTED_EDGE('',*,*,#1120,.F.);
#1537=ORIENTED_EDGE('',*,*,#1130,.T.);
#1538=ORIENTED_EDGE('',*,*,#1088,.F.);
#1539=ORIENTED_EDGE('',*,*,#1092,.F.);
#1540=ORIENTED_EDGE('',*,*,#1073,.F.);
#1541=ORIENTED_EDGE('',*,*,#1078,.F.);
#1542=ORIENTED_EDGE('',*,*,#1081,.F.);
#1543=ORIENTED_EDGE('',*,*,#1129,.T.);
#1544=ORIENTED_EDGE('',*,*,#1131,.T.);
#1545=ORIENTED_EDGE('',*,*,#1132,.T.);
#1546=ORIENTED_EDGE('',*,*,#1133,.T.);
#1547=ORIENTED_EDGE('',*,*,#1125,.T.);
#1548=ORIENTED_EDGE('',*,*,#1134,.T.);
#1549=ORIENTED_EDGE('',*,*,#1133,.F.);
#1550=ORIENTED_EDGE('',*,*,#1134,.F.);
#1551=ORIENTED_EDGE('',*,*,#1128,.T.);
#1552=ORIENTED_EDGE('',*,*,#1123,.T.);
#1553=ORIENTED_EDGE('',*,*,#1135,.T.);
#1554=ORIENTED_EDGE('',*,*,#1131,.F.);
#1555=ORIENTED_EDGE('',*,*,#1136,.T.);
#1556=ORIENTED_EDGE('',*,*,#1132,.F.);
#1557=ORIENTED_EDGE('',*,*,#1135,.F.);
#1558=ORIENTED_EDGE('',*,*,#1122,.T.);
#1559=ORIENTED_EDGE('',*,*,#1107,.T.);
#1560=ORIENTED_EDGE('',*,*,#1137,.T.);
#1561=ORIENTED_EDGE('',*,*,#1084,.T.);
#1562=ORIENTED_EDGE('',*,*,#1138,.T.);
#1563=ORIENTED_EDGE('',*,*,#1116,.T.);
#1564=ORIENTED_EDGE('',*,*,#1139,.T.);
#1565=ORIENTED_EDGE('',*,*,#1140,.T.);
#1566=ORIENTED_EDGE('',*,*,#1141,.T.);
#1567=ORIENTED_EDGE('',*,*,#1142,.T.);
#1568=ORIENTED_EDGE('',*,*,#1143,.T.);
#1569=ORIENTED_EDGE('',*,*,#1142,.F.);
#1570=ORIENTED_EDGE('',*,*,#1144,.F.);
#1571=ORIENTED_EDGE('',*,*,#1145,.F.);
#1572=ORIENTED_EDGE('',*,*,#1085,.F.);
#1573=ORIENTED_EDGE('',*,*,#1137,.F.);
#1574=ORIENTED_EDGE('',*,*,#1106,.T.);
#1575=ORIENTED_EDGE('',*,*,#1127,.F.);
#1576=ORIENTED_EDGE('',*,*,#1089,.F.);
#1577=ORIENTED_EDGE('',*,*,#1130,.F.);
#1578=ORIENTED_EDGE('',*,*,#1136,.F.);
#1579=ORIENTED_EDGE('',*,*,#1121,.F.);
#1580=ORIENTED_EDGE('',*,*,#1117,.F.);
#1581=ORIENTED_EDGE('',*,*,#1138,.F.);
#1582=ORIENTED_EDGE('',*,*,#1083,.F.);
#1583=ORIENTED_EDGE('',*,*,#1146,.F.);
#1584=ORIENTED_EDGE('',*,*,#1147,.F.);
#1585=ORIENTED_EDGE('',*,*,#1139,.F.);
#1586=ORIENTED_EDGE('',*,*,#1112,.F.);
#1587=ORIENTED_EDGE('',*,*,#1148,.T.);
#1588=ORIENTED_EDGE('',*,*,#1149,.T.);
#1589=ORIENTED_EDGE('',*,*,#1143,.F.);
#1590=ORIENTED_EDGE('',*,*,#1149,.F.);
#1591=ORIENTED_EDGE('',*,*,#1147,.T.);
#1592=ORIENTED_EDGE('',*,*,#1150,.T.);
#1593=ORIENTED_EDGE('',*,*,#1151,.T.);
#1594=ORIENTED_EDGE('',*,*,#1140,.F.);
#1595=ORIENTED_EDGE('',*,*,#1144,.T.);
#1596=ORIENTED_EDGE('',*,*,#1141,.F.);
#1597=ORIENTED_EDGE('',*,*,#1151,.F.);
#1598=ORIENTED_EDGE('',*,*,#1152,.T.);
#1599=ORIENTED_EDGE('',*,*,#1145,.T.);
#1600=ORIENTED_EDGE('',*,*,#1152,.F.);
#1601=ORIENTED_EDGE('',*,*,#1150,.F.);
#1602=ORIENTED_EDGE('',*,*,#1146,.T.);
#1603=ORIENTED_EDGE('',*,*,#1082,.T.);
#1604=ORIENTED_EDGE('',*,*,#1068,.F.);
#1605=ORIENTED_EDGE('',*,*,#1075,.T.);
#1606=ORIENTED_EDGE('',*,*,#1091,.T.);
#1607=ORIENTED_EDGE('',*,*,#1086,.T.);
#1608=ORIENTED_EDGE('',*,*,#1148,.F.);
#1609=ORIENTED_EDGE('',*,*,#1153,.F.);
#1610=ORIENTED_EDGE('',*,*,#1154,.F.);
#1611=ORIENTED_EDGE('',*,*,#1155,.F.);
#1612=ORIENTED_EDGE('',*,*,#1156,.T.);
#1613=ORIENTED_EDGE('',*,*,#1157,.F.);
#1614=ORIENTED_EDGE('',*,*,#1158,.F.);
#1615=ORIENTED_EDGE('',*,*,#1159,.F.);
#1616=ORIENTED_EDGE('',*,*,#1153,.T.);
#1617=ORIENTED_EDGE('',*,*,#1160,.T.);
#1618=ORIENTED_EDGE('',*,*,#1161,.F.);
#1619=ORIENTED_EDGE('',*,*,#1162,.F.);
#1620=ORIENTED_EDGE('',*,*,#1157,.T.);
#1621=ORIENTED_EDGE('',*,*,#1163,.T.);
#1622=ORIENTED_EDGE('',*,*,#1164,.T.);
#1623=ORIENTED_EDGE('',*,*,#1165,.F.);
#1624=ORIENTED_EDGE('',*,*,#1166,.F.);
#1625=ORIENTED_EDGE('',*,*,#1167,.F.);
#1626=ORIENTED_EDGE('',*,*,#1161,.T.);
#1627=ORIENTED_EDGE('',*,*,#1168,.T.);
#1628=ORIENTED_EDGE('',*,*,#1169,.T.);
#1629=ORIENTED_EDGE('',*,*,#1170,.F.);
#1630=ORIENTED_EDGE('',*,*,#1171,.F.);
#1631=ORIENTED_EDGE('',*,*,#1165,.T.);
#1632=ORIENTED_EDGE('',*,*,#1172,.T.);
#1633=ORIENTED_EDGE('',*,*,#1173,.T.);
#1634=ORIENTED_EDGE('',*,*,#1174,.F.);
#1635=ORIENTED_EDGE('',*,*,#1175,.F.);
#1636=ORIENTED_EDGE('',*,*,#1176,.F.);
#1637=ORIENTED_EDGE('',*,*,#1170,.T.);
#1638=ORIENTED_EDGE('',*,*,#1177,.T.);
#1639=ORIENTED_EDGE('',*,*,#1178,.F.);
#1640=ORIENTED_EDGE('',*,*,#1179,.F.);
#1641=ORIENTED_EDGE('',*,*,#1174,.T.);
#1642=ORIENTED_EDGE('',*,*,#1180,.T.);
#1643=ORIENTED_EDGE('',*,*,#1181,.T.);
#1644=ORIENTED_EDGE('',*,*,#1182,.F.);
#1645=ORIENTED_EDGE('',*,*,#1183,.F.);
#1646=ORIENTED_EDGE('',*,*,#1184,.F.);
#1647=ORIENTED_EDGE('',*,*,#1178,.T.);
#1648=ORIENTED_EDGE('',*,*,#1185,.T.);
#1649=ORIENTED_EDGE('',*,*,#1186,.F.);
#1650=ORIENTED_EDGE('',*,*,#1187,.F.);
#1651=ORIENTED_EDGE('',*,*,#1188,.F.);
#1652=ORIENTED_EDGE('',*,*,#1182,.T.);
#1653=ORIENTED_EDGE('',*,*,#1189,.T.);
#1654=ORIENTED_EDGE('',*,*,#1190,.T.);
#1655=ORIENTED_EDGE('',*,*,#1191,.F.);
#1656=ORIENTED_EDGE('',*,*,#1192,.F.);
#1657=ORIENTED_EDGE('',*,*,#1193,.F.);
#1658=ORIENTED_EDGE('',*,*,#1186,.T.);
#1659=ORIENTED_EDGE('',*,*,#1194,.T.);
#1660=ORIENTED_EDGE('',*,*,#1195,.T.);
#1661=ORIENTED_EDGE('',*,*,#1196,.F.);
#1662=ORIENTED_EDGE('',*,*,#1197,.T.);
#1663=ORIENTED_EDGE('',*,*,#1198,.T.);
#1664=ORIENTED_EDGE('',*,*,#1199,.T.);
#1665=ORIENTED_EDGE('',*,*,#1200,.T.);
#1666=ORIENTED_EDGE('',*,*,#1201,.T.);
#1667=ORIENTED_EDGE('',*,*,#1202,.T.);
#1668=ORIENTED_EDGE('',*,*,#1203,.T.);
#1669=ORIENTED_EDGE('',*,*,#1204,.T.);
#1670=ORIENTED_EDGE('',*,*,#1205,.T.);
#1671=ORIENTED_EDGE('',*,*,#1206,.T.);
#1672=ORIENTED_EDGE('',*,*,#1207,.T.);
#1673=ORIENTED_EDGE('',*,*,#1208,.T.);
#1674=ORIENTED_EDGE('',*,*,#1209,.F.);
#1675=ORIENTED_EDGE('',*,*,#1210,.T.);
#1676=ORIENTED_EDGE('',*,*,#1211,.T.);
#1677=ORIENTED_EDGE('',*,*,#1212,.T.);
#1678=ORIENTED_EDGE('',*,*,#1213,.T.);
#1679=ORIENTED_EDGE('',*,*,#1214,.T.);
#1680=ORIENTED_EDGE('',*,*,#1215,.T.);
#1681=ORIENTED_EDGE('',*,*,#1216,.T.);
#1682=ORIENTED_EDGE('',*,*,#1217,.T.);
#1683=ORIENTED_EDGE('',*,*,#1218,.T.);
#1684=ORIENTED_EDGE('',*,*,#1219,.T.);
#1685=ORIENTED_EDGE('',*,*,#1220,.T.);
#1686=ORIENTED_EDGE('',*,*,#1221,.T.);
#1687=ORIENTED_EDGE('',*,*,#1191,.T.);
#1688=ORIENTED_EDGE('',*,*,#1222,.T.);
#1689=ORIENTED_EDGE('',*,*,#1223,.F.);
#1690=ORIENTED_EDGE('',*,*,#1224,.F.);
#1691=ORIENTED_EDGE('',*,*,#1225,.F.);
#1692=ORIENTED_EDGE('',*,*,#1226,.F.);
#1693=ORIENTED_EDGE('',*,*,#1208,.F.);
#1694=ORIENTED_EDGE('',*,*,#1207,.F.);
#1695=ORIENTED_EDGE('',*,*,#1206,.F.);
#1696=ORIENTED_EDGE('',*,*,#1205,.F.);
#1697=ORIENTED_EDGE('',*,*,#1204,.F.);
#1698=ORIENTED_EDGE('',*,*,#1203,.F.);
#1699=ORIENTED_EDGE('',*,*,#1202,.F.);
#1700=ORIENTED_EDGE('',*,*,#1201,.F.);
#1701=ORIENTED_EDGE('',*,*,#1200,.F.);
#1702=ORIENTED_EDGE('',*,*,#1199,.F.);
#1703=ORIENTED_EDGE('',*,*,#1198,.F.);
#1704=ORIENTED_EDGE('',*,*,#1227,.F.);
#1705=ORIENTED_EDGE('',*,*,#1154,.T.);
#1706=ORIENTED_EDGE('',*,*,#1159,.T.);
#1707=ORIENTED_EDGE('',*,*,#1158,.T.);
#1708=ORIENTED_EDGE('',*,*,#1162,.T.);
#1709=ORIENTED_EDGE('',*,*,#1167,.T.);
#1710=ORIENTED_EDGE('',*,*,#1166,.T.);
#1711=ORIENTED_EDGE('',*,*,#1171,.T.);
#1712=ORIENTED_EDGE('',*,*,#1176,.T.);
#1713=ORIENTED_EDGE('',*,*,#1175,.T.);
#1714=ORIENTED_EDGE('',*,*,#1179,.T.);
#1715=ORIENTED_EDGE('',*,*,#1184,.T.);
#1716=ORIENTED_EDGE('',*,*,#1183,.T.);
#1717=ORIENTED_EDGE('',*,*,#1188,.T.);
#1718=ORIENTED_EDGE('',*,*,#1187,.T.);
#1719=ORIENTED_EDGE('',*,*,#1193,.T.);
#1720=ORIENTED_EDGE('',*,*,#1192,.T.);
#1721=ORIENTED_EDGE('',*,*,#1225,.T.);
#1722=ORIENTED_EDGE('',*,*,#1224,.T.);
#1723=ORIENTED_EDGE('',*,*,#1197,.F.);
#1724=ORIENTED_EDGE('',*,*,#1228,.T.);
#1725=ORIENTED_EDGE('',*,*,#1155,.T.);
#1726=ORIENTED_EDGE('',*,*,#1227,.T.);
#1727=ORIENTED_EDGE('',*,*,#1229,.F.);
#1728=ORIENTED_EDGE('',*,*,#1230,.F.);
#1729=ORIENTED_EDGE('',*,*,#1222,.F.);
#1730=ORIENTED_EDGE('',*,*,#1195,.F.);
#1731=ORIENTED_EDGE('',*,*,#1194,.F.);
#1732=ORIENTED_EDGE('',*,*,#1190,.F.);
#1733=ORIENTED_EDGE('',*,*,#1189,.F.);
#1734=ORIENTED_EDGE('',*,*,#1185,.F.);
#1735=ORIENTED_EDGE('',*,*,#1181,.F.);
#1736=ORIENTED_EDGE('',*,*,#1180,.F.);
#1737=ORIENTED_EDGE('',*,*,#1177,.F.);
#1738=ORIENTED_EDGE('',*,*,#1173,.F.);
#1739=ORIENTED_EDGE('',*,*,#1172,.F.);
#1740=ORIENTED_EDGE('',*,*,#1169,.F.);
#1741=ORIENTED_EDGE('',*,*,#1168,.F.);
#1742=ORIENTED_EDGE('',*,*,#1164,.F.);
#1743=ORIENTED_EDGE('',*,*,#1163,.F.);
#1744=ORIENTED_EDGE('',*,*,#1160,.F.);
#1745=ORIENTED_EDGE('',*,*,#1156,.F.);
#1746=ORIENTED_EDGE('',*,*,#1228,.F.);
#1747=ORIENTED_EDGE('',*,*,#1221,.F.);
#1748=ORIENTED_EDGE('',*,*,#1220,.F.);
#1749=ORIENTED_EDGE('',*,*,#1219,.F.);
#1750=ORIENTED_EDGE('',*,*,#1218,.F.);
#1751=ORIENTED_EDGE('',*,*,#1217,.F.);
#1752=ORIENTED_EDGE('',*,*,#1216,.F.);
#1753=ORIENTED_EDGE('',*,*,#1215,.F.);
#1754=ORIENTED_EDGE('',*,*,#1214,.F.);
#1755=ORIENTED_EDGE('',*,*,#1213,.F.);
#1756=ORIENTED_EDGE('',*,*,#1212,.F.);
#1757=ORIENTED_EDGE('',*,*,#1211,.F.);
#1758=ORIENTED_EDGE('',*,*,#1210,.F.);
#1759=ORIENTED_EDGE('',*,*,#1231,.F.);
#1760=ORIENTED_EDGE('',*,*,#1196,.T.);
#1761=ORIENTED_EDGE('',*,*,#1232,.F.);
#1762=ORIENTED_EDGE('',*,*,#1233,.T.);
#1763=ORIENTED_EDGE('',*,*,#1231,.T.);
#1764=ORIENTED_EDGE('',*,*,#1233,.F.);
#1765=ORIENTED_EDGE('',*,*,#1232,.T.);
#1766=ORIENTED_EDGE('',*,*,#1229,.T.);
#1767=ORIENTED_EDGE('',*,*,#1209,.T.);
#1768=ORIENTED_EDGE('',*,*,#1226,.T.);
#1769=ORIENTED_EDGE('',*,*,#1223,.T.);
#1770=ORIENTED_EDGE('',*,*,#1230,.T.);
#1771=ORIENTED_EDGE('',*,*,#1234,.T.);
#1772=ORIENTED_EDGE('',*,*,#1235,.T.);
#1773=ORIENTED_EDGE('',*,*,#1236,.F.);
#1774=ORIENTED_EDGE('',*,*,#1235,.F.);
#1775=ORIENTED_EDGE('',*,*,#1237,.T.);
#1776=ORIENTED_EDGE('',*,*,#1238,.T.);
#1777=ORIENTED_EDGE('',*,*,#1239,.F.);
#1778=ORIENTED_EDGE('',*,*,#1240,.F.);
#1779=ORIENTED_EDGE('',*,*,#1241,.T.);
#1780=ORIENTED_EDGE('',*,*,#1240,.T.);
#1781=ORIENTED_EDGE('',*,*,#1242,.F.);
#1782=ORIENTED_EDGE('',*,*,#1243,.F.);
#1783=ORIENTED_EDGE('',*,*,#1244,.T.);
#1784=ORIENTED_EDGE('',*,*,#1243,.T.);
#1785=ORIENTED_EDGE('',*,*,#1245,.F.);
#1786=ORIENTED_EDGE('',*,*,#1246,.F.);
#1787=ORIENTED_EDGE('',*,*,#1247,.T.);
#1788=ORIENTED_EDGE('',*,*,#1246,.T.);
#1789=ORIENTED_EDGE('',*,*,#1248,.F.);
#1790=ORIENTED_EDGE('',*,*,#1249,.F.);
#1791=ORIENTED_EDGE('',*,*,#1250,.T.);
#1792=ORIENTED_EDGE('',*,*,#1249,.T.);
#1793=ORIENTED_EDGE('',*,*,#1251,.F.);
#1794=ORIENTED_EDGE('',*,*,#1252,.F.);
#1795=ORIENTED_EDGE('',*,*,#1253,.T.);
#1796=ORIENTED_EDGE('',*,*,#1252,.T.);
#1797=ORIENTED_EDGE('',*,*,#1254,.F.);
#1798=ORIENTED_EDGE('',*,*,#1238,.F.);
#1799=ORIENTED_EDGE('',*,*,#1254,.T.);
#1800=ORIENTED_EDGE('',*,*,#1251,.T.);
#1801=ORIENTED_EDGE('',*,*,#1248,.T.);
#1802=ORIENTED_EDGE('',*,*,#1245,.T.);
#1803=ORIENTED_EDGE('',*,*,#1242,.T.);
#1804=ORIENTED_EDGE('',*,*,#1239,.T.);
#1805=ORIENTED_EDGE('',*,*,#1236,.T.);
#1806=ORIENTED_EDGE('',*,*,#1253,.F.);
#1807=ORIENTED_EDGE('',*,*,#1237,.F.);
#1808=ORIENTED_EDGE('',*,*,#1241,.F.);
#1809=ORIENTED_EDGE('',*,*,#1244,.F.);
#1810=ORIENTED_EDGE('',*,*,#1247,.F.);
#1811=ORIENTED_EDGE('',*,*,#1250,.F.);
#1812=ORIENTED_EDGE('',*,*,#1234,.F.);
#1813=ORIENTED_EDGE('',*,*,#1255,.T.);
#1814=ORIENTED_EDGE('',*,*,#1256,.T.);
#1815=ORIENTED_EDGE('',*,*,#1257,.T.);
#1816=ORIENTED_EDGE('',*,*,#1258,.T.);
#1817=ORIENTED_EDGE('',*,*,#1259,.T.);
#1818=ORIENTED_EDGE('',*,*,#1255,.F.);
#1819=ORIENTED_EDGE('',*,*,#1260,.T.);
#1820=ORIENTED_EDGE('',*,*,#1261,.F.);
#1821=ORIENTED_EDGE('',*,*,#1262,.F.);
#1822=ORIENTED_EDGE('',*,*,#1263,.F.);
#1823=ORIENTED_EDGE('',*,*,#1260,.F.);
#1824=ORIENTED_EDGE('',*,*,#1256,.F.);
#1825=ORIENTED_EDGE('',*,*,#1262,.T.);
#1826=ORIENTED_EDGE('',*,*,#1264,.F.);
#1827=ORIENTED_EDGE('',*,*,#1265,.F.);
#1828=ORIENTED_EDGE('',*,*,#1258,.F.);
#1829=ORIENTED_EDGE('',*,*,#1266,.T.);
#1830=ORIENTED_EDGE('',*,*,#1267,.F.);
#1831=ORIENTED_EDGE('',*,*,#1268,.T.);
#1832=ORIENTED_EDGE('',*,*,#1259,.F.);
#1833=ORIENTED_EDGE('',*,*,#1268,.F.);
#1834=ORIENTED_EDGE('',*,*,#1257,.F.);
#1835=ORIENTED_EDGE('',*,*,#1265,.T.);
#1836=ORIENTED_EDGE('',*,*,#1269,.F.);
#1837=ORIENTED_EDGE('',*,*,#1266,.F.);
#1838=ORIENTED_EDGE('',*,*,#1263,.T.);
#1839=ORIENTED_EDGE('',*,*,#1267,.T.);
#1840=ORIENTED_EDGE('',*,*,#1269,.T.);
#1841=ORIENTED_EDGE('',*,*,#1264,.T.);
#1842=ORIENTED_EDGE('',*,*,#1261,.T.);
#1843=ORIENTED_EDGE('',*,*,#1270,.T.);
#1844=ORIENTED_EDGE('',*,*,#1271,.T.);
#1845=ORIENTED_EDGE('',*,*,#1272,.F.);
#1846=ORIENTED_EDGE('',*,*,#1271,.F.);
#1847=ORIENTED_EDGE('',*,*,#1273,.T.);
#1848=ORIENTED_EDGE('',*,*,#1274,.T.);
#1849=ORIENTED_EDGE('',*,*,#1275,.F.);
#1850=ORIENTED_EDGE('',*,*,#1276,.F.);
#1851=ORIENTED_EDGE('',*,*,#1277,.T.);
#1852=ORIENTED_EDGE('',*,*,#1276,.T.);
#1853=ORIENTED_EDGE('',*,*,#1278,.F.);
#1854=ORIENTED_EDGE('',*,*,#1279,.F.);
#1855=ORIENTED_EDGE('',*,*,#1280,.T.);
#1856=ORIENTED_EDGE('',*,*,#1279,.T.);
#1857=ORIENTED_EDGE('',*,*,#1281,.F.);
#1858=ORIENTED_EDGE('',*,*,#1282,.F.);
#1859=ORIENTED_EDGE('',*,*,#1283,.T.);
#1860=ORIENTED_EDGE('',*,*,#1282,.T.);
#1861=ORIENTED_EDGE('',*,*,#1284,.F.);
#1862=ORIENTED_EDGE('',*,*,#1285,.F.);
#1863=ORIENTED_EDGE('',*,*,#1286,.T.);
#1864=ORIENTED_EDGE('',*,*,#1285,.T.);
#1865=ORIENTED_EDGE('',*,*,#1287,.F.);
#1866=ORIENTED_EDGE('',*,*,#1288,.F.);
#1867=ORIENTED_EDGE('',*,*,#1289,.T.);
#1868=ORIENTED_EDGE('',*,*,#1288,.T.);
#1869=ORIENTED_EDGE('',*,*,#1290,.F.);
#1870=ORIENTED_EDGE('',*,*,#1274,.F.);
#1871=ORIENTED_EDGE('',*,*,#1290,.T.);
#1872=ORIENTED_EDGE('',*,*,#1287,.T.);
#1873=ORIENTED_EDGE('',*,*,#1284,.T.);
#1874=ORIENTED_EDGE('',*,*,#1281,.T.);
#1875=ORIENTED_EDGE('',*,*,#1278,.T.);
#1876=ORIENTED_EDGE('',*,*,#1275,.T.);
#1877=ORIENTED_EDGE('',*,*,#1272,.T.);
#1878=ORIENTED_EDGE('',*,*,#1289,.F.);
#1879=ORIENTED_EDGE('',*,*,#1273,.F.);
#1880=ORIENTED_EDGE('',*,*,#1277,.F.);
#1881=ORIENTED_EDGE('',*,*,#1280,.F.);
#1882=ORIENTED_EDGE('',*,*,#1283,.F.);
#1883=ORIENTED_EDGE('',*,*,#1286,.F.);
#1884=ORIENTED_EDGE('',*,*,#1270,.F.);
#1885=CYLINDRICAL_SURFACE('',#2117,8.);
#1886=CYLINDRICAL_SURFACE('',#2120,10.);
#1887=CYLINDRICAL_SURFACE('',#2126,9.);
#1888=CYLINDRICAL_SURFACE('',#2132,3.22275);
#1889=CYLINDRICAL_SURFACE('',#2134,3.22275);
#1890=CYLINDRICAL_SURFACE('',#2135,3.22275);
#1891=CYLINDRICAL_SURFACE('',#2136,3.22275);
#1892=CYLINDRICAL_SURFACE('',#2137,3.22275);
#1893=CYLINDRICAL_SURFACE('',#2138,3.22275);
#1894=CYLINDRICAL_SURFACE('',#2139,3.22275);
#1895=CYLINDRICAL_SURFACE('',#2140,3.22275);
#1896=CYLINDRICAL_SURFACE('',#2141,3.933);
#1897=CYLINDRICAL_SURFACE('',#2145,3.22275);
#1898=CYLINDRICAL_SURFACE('',#2151,6.5);
#1899=CYLINDRICAL_SURFACE('',#2156,6.5);
#1900=CYLINDRICAL_SURFACE('',#2178,3.99999999999997);
#1901=CYLINDRICAL_SURFACE('',#2179,22.);
#1902=CYLINDRICAL_SURFACE('',#2180,22.);
#1903=CYLINDRICAL_SURFACE('',#2188,3.99999999999997);
#1904=CYLINDRICAL_SURFACE('',#2190,22.);
#1905=CYLINDRICAL_SURFACE('',#2192,22.);
#1906=CYLINDRICAL_SURFACE('',#2196,2.37175);
#1907=CYLINDRICAL_SURFACE('',#2198,2.37175);
#1908=CYLINDRICAL_SURFACE('',#2199,2.37175);
#1909=CYLINDRICAL_SURFACE('',#2200,2.37175);
#1910=CYLINDRICAL_SURFACE('',#2201,2.37175);
#1911=CYLINDRICAL_SURFACE('',#2202,2.37175);
#1912=CYLINDRICAL_SURFACE('',#2203,2.37175);
#1913=CYLINDRICAL_SURFACE('',#2204,2.37175);
#1914=CYLINDRICAL_SURFACE('',#2205,2.37175);
#1915=CYLINDRICAL_SURFACE('',#2206,2.37175);
#1916=CYLINDRICAL_SURFACE('',#2207,2.942);
#1917=CYLINDRICAL_SURFACE('',#2211,2.37175);
#1918=CYLINDRICAL_SURFACE('',#2216,4.);
#1919=CYLINDRICAL_SURFACE('',#2221,2.942);
#1920=CYLINDRICAL_SURFACE('',#2240,8.);
#1921=CYLINDRICAL_SURFACE('',#2247,3.933);
#1922=ADVANCED_FACE('',(#273),#1885,.F.);
#1923=ADVANCED_FACE('',(#274),#1886,.T.);
#1924=ADVANCED_FACE('',(#275,#207),#220,.T.);
#1925=ADVANCED_FACE('',(#276,#208),#221,.F.);
#1926=ADVANCED_FACE('',(#277),#1887,.T.);
#1927=ADVANCED_FACE('',(#278),#222,.T.);
#1928=ADVANCED_FACE('',(#279),#223,.F.);
#1929=ADVANCED_FACE('',(#280),#1888,.T.);
#1930=ADVANCED_FACE('',(#281),#1889,.T.);
#1931=ADVANCED_FACE('',(#282),#1890,.T.);
#1932=ADVANCED_FACE('',(#283),#1891,.T.);
#1933=ADVANCED_FACE('',(#284),#1892,.T.);
#1934=ADVANCED_FACE('',(#285),#1893,.T.);
#1935=ADVANCED_FACE('',(#286),#1894,.T.);
#1936=ADVANCED_FACE('',(#287),#1895,.T.);
#1937=ADVANCED_FACE('',(#288,#209),#1896,.T.);
#1938=ADVANCED_FACE('',(#289),#1897,.T.);
#1939=ADVANCED_FACE('',(#290),#43,.F.);
#1940=ADVANCED_FACE('',(#291),#224,.T.);
#1941=ADVANCED_FACE('',(#292),#44,.F.);
#1942=ADVANCED_FACE('',(#293),#225,.T.);
#1943=ADVANCED_FACE('',(#294),#226,.F.);
#1944=ADVANCED_FACE('',(#295),#1898,.T.);
#1945=ADVANCED_FACE('',(#296),#227,.T.);
#1946=ADVANCED_FACE('',(#297),#1899,.T.);
#1947=ADVANCED_FACE('',(#298),#228,.T.);
#1948=ADVANCED_FACE('',(#299),#229,.T.);
#1949=ADVANCED_FACE('',(#300),#230,.T.);
#1950=ADVANCED_FACE('',(#301),#231,.F.);
#1951=ADVANCED_FACE('',(#302),#232,.F.);
#1952=ADVANCED_FACE('',(#303),#233,.F.);
#1953=ADVANCED_FACE('',(#304),#45,.T.);
#1954=ADVANCED_FACE('',(#305),#234,.T.);
#1955=ADVANCED_FACE('',(#306),#235,.F.);
#1956=ADVANCED_FACE('',(#307),#46,.T.);
#1957=ADVANCED_FACE('',(#308),#236,.T.);
#1958=ADVANCED_FACE('',(#309),#237,.T.);
#1959=ADVANCED_FACE('',(#310,#210),#238,.F.);
#1960=ADVANCED_FACE('',(#311),#239,.F.);
#1961=ADVANCED_FACE('',(#312),#240,.F.);
#1962=ADVANCED_FACE('',(#313,#211),#241,.T.);
#1963=ADVANCED_FACE('',(#314),#1900,.F.);
#1964=ADVANCED_FACE('',(#315),#1901,.T.);
#1965=ADVANCED_FACE('',(#316),#1902,.T.);
#1966=ADVANCED_FACE('',(#317),#242,.T.);
#1967=ADVANCED_FACE('',(#318,#212),#243,.T.);
#1968=ADVANCED_FACE('',(#319),#244,.F.);
#1969=ADVANCED_FACE('',(#320),#245,.F.);
#1970=ADVANCED_FACE('',(#321),#1903,.F.);
#1971=ADVANCED_FACE('',(#322),#1904,.T.);
#1972=ADVANCED_FACE('',(#323),#1905,.T.);
#1973=ADVANCED_FACE('',(#324,#213),#246,.F.);
#1974=ADVANCED_FACE('',(#325),#1906,.T.);
#1975=ADVANCED_FACE('',(#326),#1907,.T.);
#1976=ADVANCED_FACE('',(#327),#1908,.T.);
#1977=ADVANCED_FACE('',(#328),#1909,.T.);
#1978=ADVANCED_FACE('',(#329),#1910,.T.);
#1979=ADVANCED_FACE('',(#330),#1911,.T.);
#1980=ADVANCED_FACE('',(#331),#1912,.T.);
#1981=ADVANCED_FACE('',(#332),#1913,.T.);
#1982=ADVANCED_FACE('',(#333),#1914,.T.);
#1983=ADVANCED_FACE('',(#334),#1915,.T.);
#1984=ADVANCED_FACE('',(#335,#214),#1916,.T.);
#1985=ADVANCED_FACE('',(#336),#1917,.T.);
#1986=ADVANCED_FACE('',(#337),#47,.F.);
#1987=ADVANCED_FACE('',(#338),#247,.T.);
#1988=ADVANCED_FACE('',(#339),#48,.F.);
#1989=ADVANCED_FACE('',(#340,#215),#248,.F.);
#1990=ADVANCED_FACE('',(#341),#1918,.T.);
#1991=ADVANCED_FACE('',(#342),#249,.T.);
#1992=ADVANCED_FACE('',(#343),#250,.F.);
#1993=ADVANCED_FACE('',(#344),#1919,.F.);
#1994=ADVANCED_FACE('',(#345),#251,.T.);
#1995=ADVANCED_FACE('',(#346),#252,.T.);
#1996=ADVANCED_FACE('',(#347),#253,.T.);
#1997=ADVANCED_FACE('',(#348),#254,.T.);
#1998=ADVANCED_FACE('',(#349),#255,.T.);
#1999=ADVANCED_FACE('',(#350),#256,.T.);
#2000=ADVANCED_FACE('',(#351,#216),#257,.T.);
#2001=ADVANCED_FACE('',(#352,#217),#258,.F.);
#2002=ADVANCED_FACE('',(#353),#259,.T.);
#2003=ADVANCED_FACE('',(#354),#260,.T.);
#2004=ADVANCED_FACE('',(#355),#261,.F.);
#2005=ADVANCED_FACE('',(#356),#262,.T.);
#2006=ADVANCED_FACE('',(#357),#1920,.T.);
#2007=ADVANCED_FACE('',(#358),#263,.T.);
#2008=ADVANCED_FACE('',(#359),#264,.T.);
#2009=ADVANCED_FACE('',(#360),#1921,.F.);
#2010=ADVANCED_FACE('',(#361),#265,.T.);
#2011=ADVANCED_FACE('',(#362),#266,.T.);
#2012=ADVANCED_FACE('',(#363),#267,.T.);
#2013=ADVANCED_FACE('',(#364),#268,.T.);
#2014=ADVANCED_FACE('',(#365),#269,.T.);
#2015=ADVANCED_FACE('',(#366),#270,.T.);
#2016=ADVANCED_FACE('',(#367,#218),#271,.T.);
#2017=ADVANCED_FACE('',(#368,#219),#272,.F.);
#2018=CLOSED_SHELL('',(#1922,#1923,#1924,#1925));
#2019=CLOSED_SHELL('',(#1926,#1927,#1928));
#2020=CLOSED_SHELL('',(#1929,#1930,#1931,#1932,#1933,#1934,#1935,#1936,
#1937,#1938,#1939,#1940,#1941,#1942,#1943));
#2021=CLOSED_SHELL('',(#1944,#1945,#1946,#1947,#1948,#1949,#1950,#1951,
#1952,#1953,#1954,#1955,#1956,#1957,#1958,#1959,#1960,#1961,#1962,#1963,
#1964,#1965,#1966,#1967,#1968,#1969,#1970,#1971,#1972,#1973));
#2022=CLOSED_SHELL('',(#1974,#1975,#1976,#1977,#1978,#1979,#1980,#1981,
#1982,#1983,#1984,#1985,#1986,#1987,#1988,#1989,#1990,#1991,#1992));
#2023=CLOSED_SHELL('',(#1993,#1994,#1995,#1996,#1997,#1998,#1999,#2000,
#2001));
#2024=CLOSED_SHELL('',(#2002,#2003,#2004,#2005,#2006,#2007,#2008));
#2025=CLOSED_SHELL('',(#2009,#2010,#2011,#2012,#2013,#2014,#2015,#2016,
#2017));
#2026=DERIVED_UNIT_ELEMENT(#2042,1.);
#2027=DERIVED_UNIT_ELEMENT(#19445,-3.);
#2028=DERIVED_UNIT_ELEMENT(#2042,1.);
#2029=DERIVED_UNIT_ELEMENT(#19445,-3.);
#2030=DERIVED_UNIT_ELEMENT(#2042,1.);
#2031=DERIVED_UNIT_ELEMENT(#19445,-3.);
#2032=DERIVED_UNIT_ELEMENT(#2042,1.);
#2033=DERIVED_UNIT_ELEMENT(#19445,-3.);
#2034=DERIVED_UNIT_ELEMENT(#2042,1.);
#2035=DERIVED_UNIT_ELEMENT(#19445,-3.);
#2036=DERIVED_UNIT_ELEMENT(#2042,1.);
#2037=DERIVED_UNIT_ELEMENT(#19445,-3.);
#2038=DERIVED_UNIT_ELEMENT(#2042,1.);
#2039=DERIVED_UNIT_ELEMENT(#19445,-3.);
#2040=DERIVED_UNIT_ELEMENT(#2042,1.);
#2041=DERIVED_UNIT_ELEMENT(#19445,-3.);
#2042=(
MASS_UNIT()
NAMED_UNIT(*)
SI_UNIT(.KILO.,.GRAM.)
);
#2043=DERIVED_UNIT((#2026,#2027));
#2044=DERIVED_UNIT((#2028,#2029));
#2045=DERIVED_UNIT((#2030,#2031));
#2046=DERIVED_UNIT((#2032,#2033));
#2047=DERIVED_UNIT((#2034,#2035));
#2048=DERIVED_UNIT((#2036,#2037));
#2049=DERIVED_UNIT((#2038,#2039));
#2050=DERIVED_UNIT((#2040,#2041));
#2051=MEASURE_REPRESENTATION_ITEM('density measure',
POSITIVE_RATIO_MEASURE(7850.),#2043);
#2052=MEASURE_REPRESENTATION_ITEM('density measure',
POSITIVE_RATIO_MEASURE(7850.),#2044);
#2053=MEASURE_REPRESENTATION_ITEM('density measure',
POSITIVE_RATIO_MEASURE(7850.),#2045);
#2054=MEASURE_REPRESENTATION_ITEM('density measure',
POSITIVE_RATIO_MEASURE(7850.),#2046);
#2055=MEASURE_REPRESENTATION_ITEM('density measure',
POSITIVE_RATIO_MEASURE(7850.),#2047);
#2056=MEASURE_REPRESENTATION_ITEM('density measure',
POSITIVE_RATIO_MEASURE(7850.),#2048);
#2057=MEASURE_REPRESENTATION_ITEM('density measure',
POSITIVE_RATIO_MEASURE(7850.),#2049);
#2058=MEASURE_REPRESENTATION_ITEM('density measure',
POSITIVE_RATIO_MEASURE(7850.),#2050);
#2059=PROPERTY_DEFINITION_REPRESENTATION(#2099,#2075);
#2060=PROPERTY_DEFINITION_REPRESENTATION(#2100,#2076);
#2061=PROPERTY_DEFINITION_REPRESENTATION(#2101,#2077);
#2062=PROPERTY_DEFINITION_REPRESENTATION(#2102,#2078);
#2063=PROPERTY_DEFINITION_REPRESENTATION(#2103,#2079);
#2064=PROPERTY_DEFINITION_REPRESENTATION(#2104,#2080);
#2065=PROPERTY_DEFINITION_REPRESENTATION(#2105,#2081);
#2066=PROPERTY_DEFINITION_REPRESENTATION(#2106,#2082);
#2067=PROPERTY_DEFINITION_REPRESENTATION(#2107,#2083);
#2068=PROPERTY_DEFINITION_REPRESENTATION(#2108,#2084);
#2069=PROPERTY_DEFINITION_REPRESENTATION(#2109,#2085);
#2070=PROPERTY_DEFINITION_REPRESENTATION(#2110,#2086);
#2071=PROPERTY_DEFINITION_REPRESENTATION(#2111,#2087);
#2072=PROPERTY_DEFINITION_REPRESENTATION(#2112,#2088);
#2073=PROPERTY_DEFINITION_REPRESENTATION(#2113,#2089);
#2074=PROPERTY_DEFINITION_REPRESENTATION(#2114,#2090);
#2075=REPRESENTATION('material name',(#2091),#19435);
#2076=REPRESENTATION('density',(#2051),#19435);
#2077=REPRESENTATION('material name',(#2092),#19436);
#2078=REPRESENTATION('density',(#2052),#19436);
#2079=REPRESENTATION('material name',(#2093),#19437);
#2080=REPRESENTATION('density',(#2053),#19437);
#2081=REPRESENTATION('material name',(#2094),#19438);
#2082=REPRESENTATION('density',(#2054),#19438);
#2083=REPRESENTATION('material name',(#2095),#19439);
#2084=REPRESENTATION('density',(#2055),#19439);
#2085=REPRESENTATION('material name',(#2096),#19440);
#2086=REPRESENTATION('density',(#2056),#19440);
#2087=REPRESENTATION('material name',(#2097),#19441);
#2088=REPRESENTATION('density',(#2057),#19441);
#2089=REPRESENTATION('material name',(#2098),#19442);
#2090=REPRESENTATION('density',(#2058),#19442);
#2091=DESCRIPTIVE_REPRESENTATION_ITEM('Steel','Steel');
#2092=DESCRIPTIVE_REPRESENTATION_ITEM('Steel','Steel');
#2093=DESCRIPTIVE_REPRESENTATION_ITEM('Steel','Steel');
#2094=DESCRIPTIVE_REPRESENTATION_ITEM('Steel','Steel');
#2095=DESCRIPTIVE_REPRESENTATION_ITEM('Steel','Steel');
#2096=DESCRIPTIVE_REPRESENTATION_ITEM('Steel','Steel');
#2097=DESCRIPTIVE_REPRESENTATION_ITEM('Steel','Steel');
#2098=DESCRIPTIVE_REPRESENTATION_ITEM('Steel','Steel');
#2099=PROPERTY_DEFINITION('material property','material name',#19485);
#2100=PROPERTY_DEFINITION('material property','density of part',#19485);
#2101=PROPERTY_DEFINITION('material property','material name',#19486);
#2102=PROPERTY_DEFINITION('material property','density of part',#19486);
#2103=PROPERTY_DEFINITION('material property','material name',#19487);
#2104=PROPERTY_DEFINITION('material property','density of part',#19487);
#2105=PROPERTY_DEFINITION('material property','material name',#19488);
#2106=PROPERTY_DEFINITION('material property','density of part',#19488);
#2107=PROPERTY_DEFINITION('material property','material name',#19489);
#2108=PROPERTY_DEFINITION('material property','density of part',#19489);
#2109=PROPERTY_DEFINITION('material property','material name',#19490);
#2110=PROPERTY_DEFINITION('material property','density of part',#19490);
#2111=PROPERTY_DEFINITION('material property','material name',#19491);
#2112=PROPERTY_DEFINITION('material property','density of part',#19491);
#2113=PROPERTY_DEFINITION('material property','material name',#19492);
#2114=PROPERTY_DEFINITION('material property','density of part',#19492);
#2115=AXIS2_PLACEMENT_3D('',#2695,#2266,#2267);
#2116=AXIS2_PLACEMENT_3D('',#2696,#2268,#2269);
#2117=AXIS2_PLACEMENT_3D('',#2697,#2270,#2271);
#2118=AXIS2_PLACEMENT_3D('',#2699,#2272,#2273);
#2119=AXIS2_PLACEMENT_3D('',#2702,#2275,#2276);
#2120=AXIS2_PLACEMENT_3D('',#2703,#2277,#2278);
#2121=AXIS2_PLACEMENT_3D('',#2705,#2279,#2280);
#2122=AXIS2_PLACEMENT_3D('',#2708,#2282,#2283);
#2123=AXIS2_PLACEMENT_3D('',#2709,#2284,#2285);
#2124=AXIS2_PLACEMENT_3D('',#2710,#2286,#2287);
#2125=AXIS2_PLACEMENT_3D('',#2711,#2288,#2289);
#2126=AXIS2_PLACEMENT_3D('',#2712,#2290,#2291);
#2127=AXIS2_PLACEMENT_3D('',#2714,#2292,#2293);
#2128=AXIS2_PLACEMENT_3D('',#2717,#2295,#2296);
#2129=AXIS2_PLACEMENT_3D('',#2718,#2297,#2298);
#2130=AXIS2_PLACEMENT_3D('',#2719,#2299,#2300);
#2131=AXIS2_PLACEMENT_3D('',#2720,#2301,#2302);
#2132=AXIS2_PLACEMENT_3D('',#2721,#2303,#2304);
#2133=AXIS2_PLACEMENT_3D('',#2839,#2306,#2307);
#2134=AXIS2_PLACEMENT_3D('',#2898,#2308,#2309);
#2135=AXIS2_PLACEMENT_3D('',#3249,#2311,#2312);
#2136=AXIS2_PLACEMENT_3D('',#3606,#2314,#2315);
#2137=AXIS2_PLACEMENT_3D('',#3965,#2317,#2318);
#2138=AXIS2_PLACEMENT_3D('',#4308,#2320,#2321);
#2139=AXIS2_PLACEMENT_3D('',#4671,#2323,#2324);
#2140=AXIS2_PLACEMENT_3D('',#5059,#2326,#2327);
#2141=AXIS2_PLACEMENT_3D('',#5456,#2329,#2330);
#2142=AXIS2_PLACEMENT_3D('',#5458,#2331,#2332);
#2143=AXIS2_PLACEMENT_3D('',#5461,#2333,#2334);
#2144=AXIS2_PLACEMENT_3D('',#7150,#2335,#2336);
#2145=AXIS2_PLACEMENT_3D('',#8731,#2337,#2338);
#2146=AXIS2_PLACEMENT_3D('',#8848,#2339,#2340);
#2147=AXIS2_PLACEMENT_3D('',#9372,#2341,#2342);
#2148=AXIS2_PLACEMENT_3D('',#9784,#2343,#2344);
#2149=AXIS2_PLACEMENT_3D('',#9785,#2345,#2346);
#2150=AXIS2_PLACEMENT_3D('',#9786,#2347,#2348);
#2151=AXIS2_PLACEMENT_3D('',#9787,#2349,#2350);
#2152=AXIS2_PLACEMENT_3D('',#9790,#2351,#2352);
#2153=AXIS2_PLACEMENT_3D('',#9794,#2354,#2355);
#2154=AXIS2_PLACEMENT_3D('',#9796,#2357,#2358);
#2155=AXIS2_PLACEMENT_3D('',#9800,#2360,#2361);
#2156=AXIS2_PLACEMENT_3D('',#9806,#2365,#2366);
#2157=AXIS2_PLACEMENT_3D('',#9810,#2368,#2369);
#2158=AXIS2_PLACEMENT_3D('',#9812,#2371,#2372);
#2159=AXIS2_PLACEMENT_3D('',#9814,#2374,#2375);
#2160=AXIS2_PLACEMENT_3D('',#9836,#2387,#2388);
#2161=AXIS2_PLACEMENT_3D('',#9839,#2391,#2392);
#2162=AXIS2_PLACEMENT_3D('',#10151,#2395,#2396);
#2163=AXIS2_PLACEMENT_3D('',#10157,#2400,#2401);
#2164=AXIS2_PLACEMENT_3D('',#10774,#2406,#2407);
#2165=AXIS2_PLACEMENT_3D('',#10778,#2410,#2411);
#2166=AXIS2_PLACEMENT_3D('',#10872,#2416,#2417);
#2167=AXIS2_PLACEMENT_3D('',#10873,#2418,#2419);
#2168=AXIS2_PLACEMENT_3D('',#10875,#2421,#2422);
#2169=AXIS2_PLACEMENT_3D('',#10879,#2424,#2425);
#2170=AXIS2_PLACEMENT_3D('',#10881,#2426,#2427);
#2171=AXIS2_PLACEMENT_3D('',#10884,#2429,#2430);
#2172=AXIS2_PLACEMENT_3D('',#10885,#2431,#2432);
#2173=AXIS2_PLACEMENT_3D('',#10888,#2435,#2436);
#2174=AXIS2_PLACEMENT_3D('',#10892,#2439,#2440);
#2175=AXIS2_PLACEMENT_3D('',#10896,#2442,#2443);
#2176=AXIS2_PLACEMENT_3D('',#10897,#2444,#2445);
#2177=AXIS2_PLACEMENT_3D('',#10899,#2446,#2447);
#2178=AXIS2_PLACEMENT_3D('',#10900,#2448,#2449);
#2179=AXIS2_PLACEMENT_3D('',#10902,#2451,#2452);
#2180=AXIS2_PLACEMENT_3D('',#10904,#2454,#2455);
#2181=AXIS2_PLACEMENT_3D('',#10906,#2457,#2458);
#2182=AXIS2_PLACEMENT_3D('',#10909,#2461,#2462);
#2183=AXIS2_PLACEMENT_3D('',#10913,#2464,#2465);
#2184=AXIS2_PLACEMENT_3D('',#10915,#2466,#2467);
#2185=AXIS2_PLACEMENT_3D('',#10918,#2469,#2470);
#2186=AXIS2_PLACEMENT_3D('',#10919,#2471,#2472);
#2187=AXIS2_PLACEMENT_3D('',#10923,#2475,#2476);
#2188=AXIS2_PLACEMENT_3D('',#10927,#2479,#2480);
#2189=AXIS2_PLACEMENT_3D('',#10929,#2481,#2482);
#2190=AXIS2_PLACEMENT_3D('',#10931,#2484,#2485);
#2191=AXIS2_PLACEMENT_3D('',#10933,#2486,#2487);
#2192=AXIS2_PLACEMENT_3D('',#10935,#2489,#2490);
#2193=AXIS2_PLACEMENT_3D('',#10936,#2491,#2492);
#2194=AXIS2_PLACEMENT_3D('',#10937,#2493,#2494);
#2195=AXIS2_PLACEMENT_3D('',#10938,#2495,#2496);
#2196=AXIS2_PLACEMENT_3D('',#10939,#2497,#2498);
#2197=AXIS2_PLACEMENT_3D('',#11048,#2500,#2501);
#2198=AXIS2_PLACEMENT_3D('',#11111,#2502,#2503);
#2199=AXIS2_PLACEMENT_3D('',#11478,#2505,#2506);
#2200=AXIS2_PLACEMENT_3D('',#11841,#2508,#2509);
#2201=AXIS2_PLACEMENT_3D('',#12101,#2511,#2512);
#2202=AXIS2_PLACEMENT_3D('',#12422,#2514,#2515);
#2203=AXIS2_PLACEMENT_3D('',#12781,#2517,#2518);
#2204=AXIS2_PLACEMENT_3D('',#13146,#2520,#2521);
#2205=AXIS2_PLACEMENT_3D('',#13401,#2523,#2524);
#2206=AXIS2_PLACEMENT_3D('',#13733,#2526,#2527);
#2207=AXIS2_PLACEMENT_3D('',#14115,#2529,#2530);
#2208=AXIS2_PLACEMENT_3D('',#14117,#2531,#2532);
#2209=AXIS2_PLACEMENT_3D('',#14120,#2533,#2534);
#2210=AXIS2_PLACEMENT_3D('',#16182,#2535,#2536);
#2211=AXIS2_PLACEMENT_3D('',#18148,#2537,#2538);
#2212=AXIS2_PLACEMENT_3D('',#18267,#2539,#2540);
#2213=AXIS2_PLACEMENT_3D('',#18821,#2541,#2542);
#2214=AXIS2_PLACEMENT_3D('',#19284,#2543,#2544);
#2215=AXIS2_PLACEMENT_3D('',#19286,#2545,#2546);
#2216=AXIS2_PLACEMENT_3D('',#19287,#2547,#2548);
#2217=AXIS2_PLACEMENT_3D('',#19289,#2549,#2550);
#2218=AXIS2_PLACEMENT_3D('',#19291,#2552,#2553);
#2219=AXIS2_PLACEMENT_3D('',#19292,#2554,#2555);
#2220=AXIS2_PLACEMENT_3D('',#19293,#2556,#2557);
#2221=AXIS2_PLACEMENT_3D('',#19294,#2558,#2559);
#2222=AXIS2_PLACEMENT_3D('',#19296,#2560,#2561);
#2223=AXIS2_PLACEMENT_3D('',#19299,#2563,#2564);
#2224=AXIS2_PLACEMENT_3D('',#19300,#2565,#2566);
#2225=AXIS2_PLACEMENT_3D('',#19309,#2571,#2572);
#2226=AXIS2_PLACEMENT_3D('',#19315,#2576,#2577);
#2227=AXIS2_PLACEMENT_3D('',#19321,#2581,#2582);
#2228=AXIS2_PLACEMENT_3D('',#19327,#2586,#2587);
#2229=AXIS2_PLACEMENT_3D('',#19333,#2591,#2592);
#2230=AXIS2_PLACEMENT_3D('',#19336,#2595,#2596);
#2231=AXIS2_PLACEMENT_3D('',#19337,#2597,#2598);
#2232=AXIS2_PLACEMENT_3D('',#19338,#2599,#2600);
#2233=AXIS2_PLACEMENT_3D('',#19339,#2601,#2602);
#2234=AXIS2_PLACEMENT_3D('',#19343,#2604,#2605);
#2235=AXIS2_PLACEMENT_3D('',#19344,#2606,#2607);
#2236=AXIS2_PLACEMENT_3D('',#19348,#2609,#2610);
#2237=AXIS2_PLACEMENT_3D('',#19349,#2611,#2612);
#2238=AXIS2_PLACEMENT_3D('',#19351,#2613,#2614);
#2239=AXIS2_PLACEMENT_3D('',#19352,#2615,#2616);
#2240=AXIS2_PLACEMENT_3D('',#19358,#2620,#2621);
#2241=AXIS2_PLACEMENT_3D('',#19360,#2622,#2623);
#2242=AXIS2_PLACEMENT_3D('',#19362,#2624,#2625);
#2243=AXIS2_PLACEMENT_3D('',#19366,#2628,#2629);
#2244=AXIS2_PLACEMENT_3D('',#19368,#2631,#2632);
#2245=AXIS2_PLACEMENT_3D('',#19370,#2634,#2635);
#2246=AXIS2_PLACEMENT_3D('',#19371,#2636,#2637);
#2247=AXIS2_PLACEMENT_3D('',#19372,#2638,#2639);
#2248=AXIS2_PLACEMENT_3D('',#19374,#2640,#2641);
#2249=AXIS2_PLACEMENT_3D('',#19377,#2643,#2644);
#2250=AXIS2_PLACEMENT_3D('',#19378,#2645,#2646);
#2251=AXIS2_PLACEMENT_3D('',#19387,#2651,#2652);
#2252=AXIS2_PLACEMENT_3D('',#19393,#2656,#2657);
#2253=AXIS2_PLACEMENT_3D('',#19399,#2661,#2662);
#2254=AXIS2_PLACEMENT_3D('',#19405,#2666,#2667);
#2255=AXIS2_PLACEMENT_3D('',#19411,#2671,#2672);
#2256=AXIS2_PLACEMENT_3D('',#19414,#2675,#2676);
#2257=AXIS2_PLACEMENT_3D('',#19415,#2677,#2678);
#2258=AXIS2_PLACEMENT_3D('',#19416,#2679,#2680);
#2259=AXIS2_PLACEMENT_3D('',#19417,#2681,#2682);
#2260=AXIS2_PLACEMENT_3D('',#19418,#2683,#2684);
#2261=AXIS2_PLACEMENT_3D('',#19419,#2685,#2686);
#2262=AXIS2_PLACEMENT_3D('',#19420,#2687,#2688);
#2263=AXIS2_PLACEMENT_3D('',#19421,#2689,#2690);
#2264=AXIS2_PLACEMENT_3D('',#19422,#2691,#2692);
#2265=AXIS2_PLACEMENT_3D('',#19423,#2693,#2694);
#2266=DIRECTION('axis',(0.,0.,1.));
#2267=DIRECTION('refdir',(1.,0.,0.));
#2268=DIRECTION('axis',(0.,0.,1.));
#2269=DIRECTION('refdir',(1.,0.,0.));
#2270=DIRECTION('center_axis',(0.,0.,1.));
#2271=DIRECTION('ref_axis',(1.,0.,0.));
#2272=DIRECTION('center_axis',(0.,0.,-1.));
#2273=DIRECTION('ref_axis',(1.,0.,0.));
#2274=DIRECTION('',(0.,0.,1.));
#2275=DIRECTION('center_axis',(0.,0.,-1.));
#2276=DIRECTION('ref_axis',(1.,0.,0.));
#2277=DIRECTION('center_axis',(0.,0.,1.));
#2278=DIRECTION('ref_axis',(1.,0.,0.));
#2279=DIRECTION('center_axis',(0.,0.,1.));
#2280=DIRECTION('ref_axis',(1.,0.,0.));
#2281=DIRECTION('',(0.,0.,-1.));
#2282=DIRECTION('center_axis',(0.,0.,1.));
#2283=DIRECTION('ref_axis',(1.,0.,0.));
#2284=DIRECTION('center_axis',(0.,0.,1.));
#2285=DIRECTION('ref_axis',(1.,0.,0.));
#2286=DIRECTION('center_axis',(0.,0.,1.));
#2287=DIRECTION('ref_axis',(1.,0.,0.));
#2288=DIRECTION('axis',(0.,0.,1.));
#2289=DIRECTION('refdir',(1.,0.,0.));
#2290=DIRECTION('center_axis',(0.,0.,1.));
#2291=DIRECTION('ref_axis',(-1.,0.,0.));
#2292=DIRECTION('center_axis',(0.,0.,1.));
#2293=DIRECTION('ref_axis',(-1.,0.,0.));
#2294=DIRECTION('',(0.,0.,-1.));
#2295=DIRECTION('center_axis',(0.,0.,1.));
#2296=DIRECTION('ref_axis',(-1.,0.,0.));
#2297=DIRECTION('center_axis',(0.,0.,1.));
#2298=DIRECTION('ref_axis',(-1.,0.,0.));
#2299=DIRECTION('center_axis',(0.,0.,1.));
#2300=DIRECTION('ref_axis',(-1.,0.,0.));
#2301=DIRECTION('axis',(0.,0.,1.));
#2302=DIRECTION('refdir',(1.,0.,0.));
#2303=DIRECTION('center_axis',(0.,0.,1.));
#2304=DIRECTION('ref_axis',(-0.853786006595012,0.52062410138462,0.));
#2305=DIRECTION('',(0.,0.,-1.));
#2306=DIRECTION('center_axis',(0.,0.,-1.));
#2307=DIRECTION('ref_axis',(-1.,-2.19773242311135E-14,0.));
#2308=DIRECTION('center_axis',(0.,0.,1.));
#2309=DIRECTION('ref_axis',(0.457827632423448,0.88904097711497,0.));
#2310=DIRECTION('',(0.,0.,-1.));
#2311=DIRECTION('center_axis',(0.,0.,1.));
#2312=DIRECTION('ref_axis',(0.457827632423448,0.88904097711497,0.));
#2313=DIRECTION('',(0.,0.,-1.));
#2314=DIRECTION('center_axis',(0.,0.,1.));
#2315=DIRECTION('ref_axis',(0.457827632423448,0.88904097711497,0.));
#2316=DIRECTION('',(0.,0.,-1.));
#2317=DIRECTION('center_axis',(0.,0.,1.));
#2318=DIRECTION('ref_axis',(0.457827632423448,0.88904097711497,0.));
#2319=DIRECTION('',(0.,0.,-1.));
#2320=DIRECTION('center_axis',(0.,0.,1.));
#2321=DIRECTION('ref_axis',(0.457827632423448,0.88904097711497,0.));
#2322=DIRECTION('',(0.,0.,-1.));
#2323=DIRECTION('center_axis',(0.,0.,1.));
#2324=DIRECTION('ref_axis',(0.457827632423448,0.88904097711497,0.));
#2325=DIRECTION('',(0.,0.,-1.));
#2326=DIRECTION('center_axis',(0.,0.,1.));
#2327=DIRECTION('ref_axis',(0.457827632423448,0.88904097711497,0.));
#2328=DIRECTION('',(0.,0.,-1.));
#2329=DIRECTION('center_axis',(0.,0.,1.));
#2330=DIRECTION('ref_axis',(-1.,0.,0.));
#2331=DIRECTION('center_axis',(0.,0.,-1.));
#2332=DIRECTION('ref_axis',(-1.,0.,0.));
#2333=DIRECTION('center_axis',(0.,0.,-1.));
#2334=DIRECTION('ref_axis',(-1.,0.,0.));
#2335=DIRECTION('center_axis',(0.,0.,-1.));
#2336=DIRECTION('ref_axis',(-1.,0.,0.));
#2337=DIRECTION('center_axis',(0.,0.,1.));
#2338=DIRECTION('ref_axis',(0.457827632423448,0.88904097711497,0.));
#2339=DIRECTION('center_axis',(0.,0.,1.));
#2340=DIRECTION('ref_axis',(-1.,-2.19773242311135E-14,0.));
#2341=DIRECTION('center_axis',(0.,0.,1.));
#2342=DIRECTION('ref_axis',(1.,0.,0.));
#2343=DIRECTION('center_axis',(0.,0.,1.));
#2344=DIRECTION('ref_axis',(-1.,0.,0.));
#2345=DIRECTION('center_axis',(0.,0.,1.));
#2346=DIRECTION('ref_axis',(-1.,0.,0.));
#2347=DIRECTION('axis',(0.,0.,1.));
#2348=DIRECTION('refdir',(1.,0.,0.));
#2349=DIRECTION('center_axis',(0.,0.,-1.));
#2350=DIRECTION('ref_axis',(-0.707106781186547,-0.707106781186548,0.));
#2351=DIRECTION('center_axis',(0.,0.,1.));
#2352=DIRECTION('ref_axis',(-0.707106781186547,-0.707106781186548,0.));
#2353=DIRECTION('',(0.,0.,1.));
#2354=DIRECTION('center_axis',(0.,0.,-1.));
#2355=DIRECTION('ref_axis',(-0.707106781186547,-0.707106781186548,0.));
#2356=DIRECTION('',(0.,0.,-1.));
#2357=DIRECTION('center_axis',(0.,0.,-1.));
#2358=DIRECTION('ref_axis',(1.,0.,0.));
#2359=DIRECTION('',(0.,1.,0.));
#2360=DIRECTION('center_axis',(0.,0.,1.));
#2361=DIRECTION('ref_axis',(-0.707106781186548,0.707106781186547,0.));
#2362=DIRECTION('',(1.,0.,0.));
#2363=DIRECTION('',(0.,1.,0.));
#2364=DIRECTION('',(1.,0.,0.));
#2365=DIRECTION('center_axis',(0.,0.,-1.));
#2366=DIRECTION('ref_axis',(-0.707106781186548,0.707106781186547,0.));
#2367=DIRECTION('',(0.,0.,1.));
#2368=DIRECTION('center_axis',(0.,0.,-1.));
#2369=DIRECTION('ref_axis',(-0.707106781186548,0.707106781186547,0.));
#2370=DIRECTION('',(0.,0.,-1.));
#2371=DIRECTION('center_axis',(-1.,0.,0.));
#2372=DIRECTION('ref_axis',(0.,0.,-1.));
#2373=DIRECTION('',(0.,1.,0.));
#2374=DIRECTION('center_axis',(0.,0.,1.));
#2375=DIRECTION('ref_axis',(-1.,0.,0.));
#2376=DIRECTION('',(0.,1.,0.));
#2377=DIRECTION('',(-1.,0.,0.));
#2378=DIRECTION('',(-1.,0.,0.));
#2379=DIRECTION('',(0.,1.,0.));
#2380=DIRECTION('',(-1.,0.,0.));
#2381=DIRECTION('',(0.,-1.,0.));
#2382=DIRECTION('',(-1.,0.,0.));
#2383=DIRECTION('',(0.,-1.,0.));
#2384=DIRECTION('',(-1.,0.,0.));
#2385=DIRECTION('',(0.,-1.,0.));
#2386=DIRECTION('',(1.,0.,0.));
#2387=DIRECTION('center_axis',(1.,0.,0.));
#2388=DIRECTION('ref_axis',(0.,0.,1.));
#2389=DIRECTION('',(0.,0.,1.));
#2390=DIRECTION('',(0.,0.,1.));
#2391=DIRECTION('center_axis',(0.,1.,0.));
#2392=DIRECTION('ref_axis',(-1.,0.,0.));
#2393=DIRECTION('',(0.,0.,1.));
#2394=DIRECTION('',(0.86390887084174,0.,-0.503648153854405));
#2395=DIRECTION('center_axis',(1.,0.,0.));
#2396=DIRECTION('ref_axis',(0.,1.,0.));
#2397=DIRECTION('',(0.,1.,0.));
#2398=DIRECTION('',(0.,0.,1.));
#2399=DIRECTION('',(-1.20956479566685E-15,-1.,0.));
#2400=DIRECTION('center_axis',(0.,-1.,0.));
#2401=DIRECTION('ref_axis',(1.,0.,0.));
#2402=DIRECTION('',(-0.86390887084174,0.,0.503648153854405));
#2403=DIRECTION('',(0.,1.,0.));
#2404=DIRECTION('',(0.,1.,0.));
#2405=DIRECTION('',(0.,1.,0.));
#2406=DIRECTION('center_axis',(0.503648153854405,0.,0.86390887084174));
#2407=DIRECTION('ref_axis',(0.86390887084174,0.,-0.503648153854405));
#2408=DIRECTION('',(0.,1.,0.));
#2409=DIRECTION('',(0.86390887084174,0.,-0.503648153854405));
#2410=DIRECTION('center_axis',(0.,1.,0.));
#2411=DIRECTION('ref_axis',(-1.,0.,0.));
#2412=DIRECTION('',(0.,0.,1.));
#2413=DIRECTION('',(0.86390887084174,0.,-0.503648153854405));
#2414=DIRECTION('',(0.,1.,0.));
#2415=DIRECTION('',(0.,1.,0.));
#2416=DIRECTION('center_axis',(0.503648153854405,0.,0.86390887084174));
#2417=DIRECTION('ref_axis',(0.86390887084174,0.,-0.503648153854405));
#2418=DIRECTION('center_axis',(0.,1.,0.));
#2419=DIRECTION('ref_axis',(-1.,0.,0.));
#2420=DIRECTION('',(0.,0.,-1.));
#2421=DIRECTION('center_axis',(0.,1.,0.));
#2422=DIRECTION('ref_axis',(1.,0.,0.));
#2423=DIRECTION('',(0.,0.,1.));
#2424=DIRECTION('center_axis',(0.,1.,0.));
#2425=DIRECTION('ref_axis',(-1.00929365875014E-15,0.,1.));
#2426=DIRECTION('center_axis',(0.,1.,0.));
#2427=DIRECTION('ref_axis',(-1.,0.,4.84460956200068E-15));
#2428=DIRECTION('',(0.,0.,-1.));
#2429=DIRECTION('center_axis',(0.,-1.,0.));
#2430=DIRECTION('ref_axis',(1.,0.,0.));
#2431=DIRECTION('center_axis',(0.,1.,0.));
#2432=DIRECTION('ref_axis',(1.,0.,0.));
#2433=DIRECTION('',(0.,0.,-1.));
#2434=DIRECTION('',(0.,0.,1.));
#2435=DIRECTION('center_axis',(1.,0.,0.));
#2436=DIRECTION('ref_axis',(0.,0.,-1.));
#2437=DIRECTION('',(0.,-1.,0.));
#2438=DIRECTION('',(0.,0.,1.));
#2439=DIRECTION('center_axis',(0.,1.,0.));
#2440=DIRECTION('ref_axis',(1.,0.,0.));
#2441=DIRECTION('',(0.,0.,-1.));
#2442=DIRECTION('center_axis',(0.,1.,0.));
#2443=DIRECTION('ref_axis',(-1.,0.,4.84460956200068E-15));
#2444=DIRECTION('center_axis',(0.,1.,0.));
#2445=DIRECTION('ref_axis',(-1.00929365875014E-15,0.,1.));
#2446=DIRECTION('center_axis',(0.,-1.,0.));
#2447=DIRECTION('ref_axis',(1.,0.,0.));
#2448=DIRECTION('center_axis',(0.,1.,0.));
#2449=DIRECTION('ref_axis',(1.,0.,0.));
#2450=DIRECTION('',(0.,1.,0.));
#2451=DIRECTION('center_axis',(0.,1.,0.));
#2452=DIRECTION('ref_axis',(-1.,0.,4.84460956200068E-15));
#2453=DIRECTION('',(0.,1.,0.));
#2454=DIRECTION('center_axis',(0.,1.,0.));
#2455=DIRECTION('ref_axis',(-1.00929365875014E-15,0.,1.));
#2456=DIRECTION('',(0.,1.,0.));
#2457=DIRECTION('center_axis',(0.,1.,0.));
#2458=DIRECTION('ref_axis',(1.,0.,0.));
#2459=DIRECTION('',(0.,0.,-1.));
#2460=DIRECTION('',(0.,0.,1.));
#2461=DIRECTION('center_axis',(0.,1.,0.));
#2462=DIRECTION('ref_axis',(1.,0.,0.));
#2463=DIRECTION('',(0.,0.,1.));
#2464=DIRECTION('center_axis',(0.,1.,0.));
#2465=DIRECTION('ref_axis',(-1.,0.,4.84460956200068E-15));
#2466=DIRECTION('center_axis',(0.,1.,0.));
#2467=DIRECTION('ref_axis',(-1.00929365875014E-15,0.,1.));
#2468=DIRECTION('',(0.,0.,-1.));
#2469=DIRECTION('center_axis',(0.,-1.,0.));
#2470=DIRECTION('ref_axis',(1.,0.,0.));
#2471=DIRECTION('center_axis',(-1.,0.,0.));
#2472=DIRECTION('ref_axis',(0.,0.,1.));
#2473=DIRECTION('',(0.,1.,0.));
#2474=DIRECTION('',(0.,0.,1.));
#2475=DIRECTION('center_axis',(1.,0.,0.));
#2476=DIRECTION('ref_axis',(0.,0.,-1.));
#2477=DIRECTION('',(0.,0.,-1.));
#2478=DIRECTION('',(0.,-1.,0.));
#2479=DIRECTION('center_axis',(0.,1.,0.));
#2480=DIRECTION('ref_axis',(1.,0.,0.));
#2481=DIRECTION('center_axis',(0.,-1.,0.));
#2482=DIRECTION('ref_axis',(1.,0.,0.));
#2483=DIRECTION('',(0.,1.,0.));
#2484=DIRECTION('center_axis',(0.,1.,0.));
#2485=DIRECTION('ref_axis',(-1.,0.,4.84460956200068E-15));
#2486=DIRECTION('center_axis',(0.,1.,0.));
#2487=DIRECTION('ref_axis',(-1.,0.,4.84460956200068E-15));
#2488=DIRECTION('',(0.,1.,0.));
#2489=DIRECTION('center_axis',(0.,1.,0.));
#2490=DIRECTION('ref_axis',(-1.00929365875014E-15,0.,1.));
#2491=DIRECTION('center_axis',(0.,1.,0.));
#2492=DIRECTION('ref_axis',(-1.00929365875014E-15,0.,1.));
#2493=DIRECTION('center_axis',(0.,1.,0.));
#2494=DIRECTION('ref_axis',(1.,0.,0.));
#2495=DIRECTION('axis',(0.,0.,1.));
#2496=DIRECTION('refdir',(1.,0.,0.));
#2497=DIRECTION('center_axis',(0.,0.,1.));
#2498=DIRECTION('ref_axis',(-0.457964771069041,-0.888970341721073,0.));
#2499=DIRECTION('',(0.,0.,-1.));
#2500=DIRECTION('center_axis',(0.,0.,-1.));
#2501=DIRECTION('ref_axis',(1.,5.97970744629653E-14,0.));
#2502=DIRECTION('center_axis',(0.,0.,1.));
#2503=DIRECTION('ref_axis',(-0.457964771069041,-0.888970341721073,0.));
#2504=DIRECTION('',(0.,0.,-1.));
#2505=DIRECTION('center_axis',(0.,0.,1.));
#2506=DIRECTION('ref_axis',(-0.457964771069041,-0.888970341721073,0.));
#2507=DIRECTION('',(0.,0.,-1.));
#2508=DIRECTION('center_axis',(0.,0.,1.));
#2509=DIRECTION('ref_axis',(-0.457964771069041,-0.888970341721073,0.));
#2510=DIRECTION('',(0.,0.,-1.));
#2511=DIRECTION('center_axis',(0.,0.,1.));
#2512=DIRECTION('ref_axis',(-0.457964771069041,-0.888970341721073,0.));
#2513=DIRECTION('',(0.,0.,-1.));
#2514=DIRECTION('center_axis',(0.,0.,1.));
#2515=DIRECTION('ref_axis',(-0.457964771069041,-0.888970341721073,0.));
#2516=DIRECTION('',(0.,0.,-1.));
#2517=DIRECTION('center_axis',(0.,0.,1.));
#2518=DIRECTION('ref_axis',(-0.457964771069041,-0.888970341721073,0.));
#2519=DIRECTION('',(0.,0.,-1.));
#2520=DIRECTION('center_axis',(0.,0.,1.));
#2521=DIRECTION('ref_axis',(-0.457964771069041,-0.888970341721073,0.));
#2522=DIRECTION('',(0.,0.,-1.));
#2523=DIRECTION('center_axis',(0.,0.,1.));
#2524=DIRECTION('ref_axis',(-0.457964771069041,-0.888970341721073,0.));
#2525=DIRECTION('',(0.,0.,-1.));
#2526=DIRECTION('center_axis',(0.,0.,1.));
#2527=DIRECTION('ref_axis',(-0.457964771069041,-0.888970341721073,0.));
#2528=DIRECTION('',(0.,0.,-1.));
#2529=DIRECTION('center_axis',(0.,0.,1.));
#2530=DIRECTION('ref_axis',(1.,0.,0.));
#2531=DIRECTION('center_axis',(0.,0.,1.));
#2532=DIRECTION('ref_axis',(1.,0.,0.));
#2533=DIRECTION('center_axis',(0.,0.,-1.));
#2534=DIRECTION('ref_axis',(1.,0.,0.));
#2535=DIRECTION('center_axis',(0.,0.,1.));
#2536=DIRECTION('ref_axis',(1.,0.,0.));
#2537=DIRECTION('center_axis',(0.,0.,1.));
#2538=DIRECTION('ref_axis',(-0.457964771069041,-0.888970341721073,0.));
#2539=DIRECTION('center_axis',(0.,0.,1.));
#2540=DIRECTION('ref_axis',(1.,5.97970744629653E-14,0.));
#2541=DIRECTION('center_axis',(0.,0.,1.));
#2542=DIRECTION('ref_axis',(1.,0.,0.));
#2543=DIRECTION('center_axis',(0.,0.,-1.));
#2544=DIRECTION('ref_axis',(1.,0.,0.));
#2545=DIRECTION('center_axis',(0.,0.,-1.));
#2546=DIRECTION('ref_axis',(1.,0.,0.));
#2547=DIRECTION('center_axis',(0.,0.,-1.));
#2548=DIRECTION('ref_axis',(1.,0.,0.));
#2549=DIRECTION('center_axis',(0.,0.,-1.));
#2550=DIRECTION('ref_axis',(1.,0.,0.));
#2551=DIRECTION('',(0.,0.,1.));
#2552=DIRECTION('center_axis',(0.,0.,-1.));
#2553=DIRECTION('ref_axis',(1.,0.,0.));
#2554=DIRECTION('center_axis',(0.,0.,-1.));
#2555=DIRECTION('ref_axis',(1.,0.,0.));
#2556=DIRECTION('axis',(0.,0.,1.));
#2557=DIRECTION('refdir',(1.,0.,0.));
#2558=DIRECTION('center_axis',(0.,0.,1.));
#2559=DIRECTION('ref_axis',(-1.,0.,0.));
#2560=DIRECTION('center_axis',(0.,0.,-1.));
#2561=DIRECTION('ref_axis',(-1.,0.,0.));
#2562=DIRECTION('',(0.,0.,1.));
#2563=DIRECTION('center_axis',(0.,0.,-1.));
#2564=DIRECTION('ref_axis',(-1.,0.,0.));
#2565=DIRECTION('center_axis',(-0.866025403784439,-0.5,0.));
#2566=DIRECTION('ref_axis',(0.5,-0.866025403784439,0.));
#2567=DIRECTION('',(0.5,-0.866025403784439,0.));
#2568=DIRECTION('',(0.,0.,1.));
#2569=DIRECTION('',(0.5,-0.866025403784439,0.));
#2570=DIRECTION('',(0.,0.,1.));
#2571=DIRECTION('center_axis',(-0.866025403784439,0.5,0.));
#2572=DIRECTION('ref_axis',(-0.5,-0.866025403784439,0.));
#2573=DIRECTION('',(-0.5,-0.866025403784439,0.));
#2574=DIRECTION('',(-0.5,-0.866025403784439,0.));
#2575=DIRECTION('',(0.,0.,1.));
#2576=DIRECTION('center_axis',(1.20185167898973E-16,1.,0.));
#2577=DIRECTION('ref_axis',(-1.,1.20185167898973E-16,0.));
#2578=DIRECTION('',(-1.,1.20185167898973E-16,0.));
#2579=DIRECTION('',(-1.,1.20185167898973E-16,0.));
#2580=DIRECTION('',(0.,0.,1.));
#2581=DIRECTION('center_axis',(0.866025403784439,0.5,0.));
#2582=DIRECTION('ref_axis',(-0.5,0.866025403784439,0.));
#2583=DIRECTION('',(-0.5,0.866025403784439,0.));
#2584=DIRECTION('',(-0.5,0.866025403784439,0.));
#2585=DIRECTION('',(0.,0.,1.));
#2586=DIRECTION('center_axis',(0.866025403784439,-0.5,0.));
#2587=DIRECTION('ref_axis',(0.5,0.866025403784439,0.));
#2588=DIRECTION('',(0.5,0.866025403784439,0.));
#2589=DIRECTION('',(0.5,0.866025403784439,0.));
#2590=DIRECTION('',(0.,0.,1.));
#2591=DIRECTION('center_axis',(2.40370335797945E-16,-1.,0.));
#2592=DIRECTION('ref_axis',(1.,2.40370335797945E-16,0.));
#2593=DIRECTION('',(1.,2.40370335797945E-16,0.));
#2594=DIRECTION('',(1.,2.40370335797945E-16,0.));
#2595=DIRECTION('center_axis',(0.,0.,1.));
#2596=DIRECTION('ref_axis',(-1.,0.,0.));
#2597=DIRECTION('center_axis',(0.,0.,1.));
#2598=DIRECTION('ref_axis',(-1.,0.,0.));
#2599=DIRECTION('axis',(0.,0.,1.));
#2600=DIRECTION('refdir',(1.,0.,0.));
#2601=DIRECTION('center_axis',(0.,0.,-1.));
#2602=DIRECTION('ref_axis',(1.,0.,0.));
#2603=DIRECTION('',(1.,0.,0.));
#2604=DIRECTION('center_axis',(0.,0.,-1.));
#2605=DIRECTION('ref_axis',(1.,0.,0.));
#2606=DIRECTION('center_axis',(0.,0.,-1.));
#2607=DIRECTION('ref_axis',(1.,0.,0.));
#2608=DIRECTION('',(-1.,0.,0.));
#2609=DIRECTION('center_axis',(0.,0.,-1.));
#2610=DIRECTION('ref_axis',(1.,0.,0.));
#2611=DIRECTION('center_axis',(0.,0.,-1.));
#2612=DIRECTION('ref_axis',(1.,0.,0.));
#2613=DIRECTION('center_axis',(0.,0.,1.));
#2614=DIRECTION('ref_axis',(1.,0.,0.));
#2615=DIRECTION('center_axis',(0.,-1.,0.));
#2616=DIRECTION('ref_axis',(-1.,0.,0.));
#2617=DIRECTION('',(0.,0.,-1.));
#2618=DIRECTION('',(-1.,0.,0.));
#2619=DIRECTION('',(0.,0.,-1.));
#2620=DIRECTION('center_axis',(0.,0.,-1.));
#2621=DIRECTION('ref_axis',(1.,0.,0.));
#2622=DIRECTION('center_axis',(0.,0.,-1.));
#2623=DIRECTION('ref_axis',(1.,0.,0.));
#2624=DIRECTION('center_axis',(0.,0.,-1.));
#2625=DIRECTION('ref_axis',(1.,0.,0.));
#2626=DIRECTION('',(0.,0.,-1.));
#2627=DIRECTION('',(0.,0.,-1.));
#2628=DIRECTION('center_axis',(0.,0.,-1.));
#2629=DIRECTION('ref_axis',(1.,0.,0.));
#2630=DIRECTION('',(0.,0.,1.));
#2631=DIRECTION('center_axis',(0.,1.,0.));
#2632=DIRECTION('ref_axis',(1.,0.,0.));
#2633=DIRECTION('',(1.,0.,0.));
#2634=DIRECTION('center_axis',(0.,0.,-1.));
#2635=DIRECTION('ref_axis',(1.,0.,0.));
#2636=DIRECTION('axis',(0.,0.,1.));
#2637=DIRECTION('refdir',(1.,0.,0.));
#2638=DIRECTION('center_axis',(0.,0.,-1.));
#2639=DIRECTION('ref_axis',(1.,0.,0.));
#2640=DIRECTION('center_axis',(0.,0.,1.));
#2641=DIRECTION('ref_axis',(1.,0.,0.));
#2642=DIRECTION('',(0.,0.,-1.));
#2643=DIRECTION('center_axis',(0.,0.,1.));
#2644=DIRECTION('ref_axis',(1.,0.,0.));
#2645=DIRECTION('center_axis',(-0.866025403784439,0.499999999999999,0.));
#2646=DIRECTION('ref_axis',(0.499999999999999,0.866025403784439,0.));
#2647=DIRECTION('',(0.499999999999999,0.866025403784439,0.));
#2648=DIRECTION('',(0.,0.,-1.));
#2649=DIRECTION('',(0.499999999999999,0.866025403784439,0.));
#2650=DIRECTION('',(0.,0.,-1.));
#2651=DIRECTION('center_axis',(-0.866025403784438,-0.500000000000001,0.));
#2652=DIRECTION('ref_axis',(-0.500000000000001,0.866025403784438,0.));
#2653=DIRECTION('',(-0.500000000000001,0.866025403784438,0.));
#2654=DIRECTION('',(-0.500000000000001,0.866025403784438,0.));
#2655=DIRECTION('',(0.,0.,-1.));
#2656=DIRECTION('center_axis',(4.93050094494016E-16,-1.,0.));
#2657=DIRECTION('ref_axis',(-1.,-4.93050094494016E-16,0.));
#2658=DIRECTION('',(-1.,-4.93050094494016E-16,0.));
#2659=DIRECTION('',(-1.,-4.93050094494016E-16,0.));
#2660=DIRECTION('',(0.,0.,-1.));
#2661=DIRECTION('center_axis',(0.866025403784439,-0.5,0.));
#2662=DIRECTION('ref_axis',(-0.5,-0.866025403784439,0.));
#2663=DIRECTION('',(-0.5,-0.866025403784439,0.));
#2664=DIRECTION('',(-0.5,-0.866025403784439,0.));
#2665=DIRECTION('',(0.,0.,-1.));
#2666=DIRECTION('center_axis',(0.866025403784439,0.5,0.));
#2667=DIRECTION('ref_axis',(0.5,-0.866025403784439,0.));
#2668=DIRECTION('',(0.5,-0.866025403784439,0.));
#2669=DIRECTION('',(0.5,-0.866025403784439,0.));
#2670=DIRECTION('',(0.,0.,-1.));
#2671=DIRECTION('center_axis',(-6.57400125992021E-16,1.,0.));
#2672=DIRECTION('ref_axis',(1.,6.57400125992021E-16,0.));
#2673=DIRECTION('',(1.,6.57400125992021E-16,0.));
#2674=DIRECTION('',(1.,6.57400125992021E-16,0.));
#2675=DIRECTION('center_axis',(0.,0.,-1.));
#2676=DIRECTION('ref_axis',(1.,0.,0.));
#2677=DIRECTION('center_axis',(0.,0.,-1.));
#2678=DIRECTION('ref_axis',(1.,0.,0.));
#2679=DIRECTION('',(0.,0.,1.));
#2680=DIRECTION('',(1.,0.,0.));
#2681=DIRECTION('',(0.,0.,1.));
#2682=DIRECTION('',(1.,0.,0.));
#2683=DIRECTION('',(0.,0.,1.));
#2684=DIRECTION('',(1.,0.,0.));
#2685=DIRECTION('',(0.,0.,1.));
#2686=DIRECTION('',(1.,0.,0.));
#2687=DIRECTION('',(0.,0.,1.));
#2688=DIRECTION('',(1.,0.,0.));
#2689=DIRECTION('',(0.,0.,1.));
#2690=DIRECTION('',(1.,0.,0.));
#2691=DIRECTION('',(0.,0.,1.));
#2692=DIRECTION('',(1.,0.,0.));
#2693=DIRECTION('',(0.,0.,1.));
#2694=DIRECTION('',(1.,0.,0.));
#2695=CARTESIAN_POINT('',(0.,0.,0.));
#2696=CARTESIAN_POINT('',(0.,0.,0.));
#2697=CARTESIAN_POINT('Origin',(0.,0.,0.));
#2698=CARTESIAN_POINT('',(-8.,-9.79717439317882E-16,0.));
#2699=CARTESIAN_POINT('Origin',(0.,0.,0.));
#2700=CARTESIAN_POINT('',(-8.,-9.79717439317882E-16,170.));
#2701=CARTESIAN_POINT('',(-8.,-9.79717439317883E-16,0.));
#2702=CARTESIAN_POINT('Origin',(0.,0.,170.));
#2703=CARTESIAN_POINT('Origin',(0.,0.,0.));
#2704=CARTESIAN_POINT('',(-10.,-1.22464679914735E-15,170.));
#2705=CARTESIAN_POINT('Origin',(0.,0.,170.));
#2706=CARTESIAN_POINT('',(-10.,-1.22464679914735E-15,0.));
#2707=CARTESIAN_POINT('',(-10.,-1.22464679914735E-15,0.));
#2708=CARTESIAN_POINT('Origin',(0.,0.,0.));
#2709=CARTESIAN_POINT('Origin',(0.,0.,170.));
#2710=CARTESIAN_POINT('Origin',(0.,0.,0.));
#2711=CARTESIAN_POINT('',(0.,0.,0.));
#2712=CARTESIAN_POINT('Origin',(0.,0.,170.));
#2713=CARTESIAN_POINT('',(9.,1.10218211923262E-15,177.));
#2714=CARTESIAN_POINT('Origin',(0.,0.,177.));
#2715=CARTESIAN_POINT('',(9.,1.10218211923262E-15,170.));
#2716=CARTESIAN_POINT('',(9.,1.10218211923262E-15,170.));
#2717=CARTESIAN_POINT('Origin',(0.,0.,170.));
#2718=CARTESIAN_POINT('Origin',(0.,0.,177.));
#2719=CARTESIAN_POINT('Origin',(0.,0.,170.));
#2720=CARTESIAN_POINT('',(0.,0.,0.));
#2721=CARTESIAN_POINT('Origin',(0.,0.,294.689226550727));
#2722=CARTESIAN_POINT('',(-1.47546400239267,-2.86515680899727,297.653713253152));
#2723=CARTESIAN_POINT('',(-1.47546398584926,-2.86515681751659,297.410170442659));
#2724=CARTESIAN_POINT('',(-1.47546400239267,-2.86515680899727,294.689226550727));
#2725=CARTESIAN_POINT('',(1.87151685390576,2.62365055372218,297.000096128141));
#2726=CARTESIAN_POINT('Ctrl Pts',(1.87151685390576,2.62365055372218,297.000096128141));
#2727=CARTESIAN_POINT('Ctrl Pts',(1.79141615285366,2.68078842668167,297.00620095976));
#2728=CARTESIAN_POINT('Ctrl Pts',(1.70855111526434,2.7343581154886,297.012305791378));
#2729=CARTESIAN_POINT('Ctrl Pts',(1.62327730492518,2.78407764866838,297.018410622997));
#2730=CARTESIAN_POINT('Ctrl Pts',(1.53811042861501,2.83373483316243,297.024507799109));
#2731=CARTESIAN_POINT('Ctrl Pts',(1.45054116169697,2.87955123245278,297.030604975221));
#2732=CARTESIAN_POINT('Ctrl Pts',(1.3609557972031,2.9212868535218,297.036702151332));
#2733=CARTESIAN_POINT('Ctrl Pts',(1.27145830627926,2.96298153645274,297.042793346772));
#2734=CARTESIAN_POINT('Ctrl Pts',(1.179949049884,3.00060321142747,297.048884542213));
#2735=CARTESIAN_POINT('Ctrl Pts',(1.08683978303569,3.03395729180734,297.054975737653));
#2736=CARTESIAN_POINT('Ctrl Pts',(0.993779731326844,3.06729374208686,297.061063713446));
#2737=CARTESIAN_POINT('Ctrl Pts',(0.899121766051749,3.096366927626,297.067151689238));
#2738=CARTESIAN_POINT('Ctrl Pts',(0.80329768648275,3.12103034099181,297.073239665031));
#2739=CARTESIAN_POINT('Ctrl Pts',(0.707497314123379,3.14568765254362,297.079326134637));
#2740=CARTESIAN_POINT('Ctrl Pts',(0.610531830865964,3.16593724870124,297.085412604243));
#2741=CARTESIAN_POINT('Ctrl Pts',(0.512847160816357,3.18168278622219,297.09149907385));
#2742=CARTESIAN_POINT('Ctrl Pts',(0.415159192462197,3.19742885538826,297.097585748964));
#2743=CARTESIAN_POINT('Ctrl Pts',(0.316752428147877,3.20867049459657,297.103672424079));
#2744=CARTESIAN_POINT('Ctrl Pts',(0.21808078403911,3.21536286196953,297.109759099194));
#2745=CARTESIAN_POINT('Ctrl Pts',(0.119317279639045,3.2220614597324,297.115851440818));
#2746=CARTESIAN_POINT('Ctrl Pts',(0.0202888472946114,3.22420229773245,297.121943782441));
#2747=CARTESIAN_POINT('Ctrl Pts',(-0.0785480134665766,3.22179263331464,
297.128036124065));
#2748=CARTESIAN_POINT('Ctrl Pts',(-0.177431840313444,3.21938182385332,297.134131360696));
#2749=CARTESIAN_POINT('Ctrl Pts',(-0.276123470897804,3.21241623846137,297.140226597327));
#2750=CARTESIAN_POINT('Ctrl Pts',(-0.374171112763951,3.20095509822818,297.146321833958));
#2751=CARTESIAN_POINT('Ctrl Pts',(-0.472375829059162,3.18947559700207,297.152426835289));
#2752=CARTESIAN_POINT('Ctrl Pts',(-0.569934057389595,3.17348622911528,297.15853183662));
#2753=CARTESIAN_POINT('Ctrl Pts',(-0.66640380079212,3.1530974512041,297.164636837951));
#2754=CARTESIAN_POINT('Ctrl Pts',(-0.743036967641216,3.13690111270037,297.169486499297));
#2755=CARTESIAN_POINT('Ctrl Pts',(-0.818983426118032,3.11792963437914,297.174336160643));
#2756=CARTESIAN_POINT('Ctrl Pts',(-0.89402967360142,3.09626040655823,297.179185821989));
#2757=CARTESIAN_POINT('Ctrl Pts',(-0.989823629542428,3.06860038190994,297.185376248038));
#2758=CARTESIAN_POINT('Ctrl Pts',(-1.08448985773541,3.0364452542115,297.191566674086));
#2759=CARTESIAN_POINT('Ctrl Pts',(-1.17757729863649,2.99990487653125,297.197757100135));
#2760=CARTESIAN_POINT('Ctrl Pts',(-1.27054427470928,2.9634117858994,297.203939515129));
#2761=CARTESIAN_POINT('Ctrl Pts',(-1.36193612688466,2.92254488352808,297.210121930123));
#2762=CARTESIAN_POINT('Ctrl Pts',(-1.45131602364403,2.87746405051637,297.216304345117));
#2763=CARTESIAN_POINT('Ctrl Pts',(-1.5406061879105,2.83242847617775,297.222480553306));
#2764=CARTESIAN_POINT('Ctrl Pts',(-1.62788803009054,2.78318757691115,297.228656761496));
#2765=CARTESIAN_POINT('Ctrl Pts',(-1.71274467983952,2.7299493079875,297.234832969686));
#2766=CARTESIAN_POINT('Ctrl Pts',(-1.79754448300981,2.67674670407599,297.241005040353));
#2767=CARTESIAN_POINT('Ctrl Pts',(-1.87992195979798,2.61955228375788,297.24717711102));
#2768=CARTESIAN_POINT('Ctrl Pts',(-1.95948561107439,2.55861949154079,297.253349181687));
#2769=CARTESIAN_POINT('Ctrl Pts',(-2.03902221220878,2.49770741532473,297.259519153967));
#2770=CARTESIAN_POINT('Ctrl Pts',(-2.11574654703192,2.43305975523258,297.265689126246));
#2771=CARTESIAN_POINT('Ctrl Pts',(-2.18929756661504,2.36497224662648,297.271859098526));
#2772=CARTESIAN_POINT('Ctrl Pts',(-2.26284290673704,2.29688999560021,297.278028594372));
#2773=CARTESIAN_POINT('Ctrl Pts',(-2.33321510254691,2.22536871743231,297.284198090219));
#2774=CARTESIAN_POINT('Ctrl Pts',(-2.4000882941973,2.15074260258104,297.290367586065));
#2775=CARTESIAN_POINT('Ctrl Pts',(-2.46697389341984,2.07610264168952,297.296538226593));
#2776=CARTESIAN_POINT('Ctrl Pts',(-2.5303589108648,1.99835702081822,297.30270886712));
#2777=CARTESIAN_POINT('Ctrl Pts',(-2.58995692026528,1.91787400881027,297.308879507648));
#2778=CARTESIAN_POINT('Ctrl Pts',(-2.64961799436772,1.83730583226049,297.315056677749));
#2779=CARTESIAN_POINT('Ctrl Pts',(-2.70548380233446,1.75399482833522,297.321233847851));
#2780=CARTESIAN_POINT('Ctrl Pts',(-2.75731060812822,1.66833922593806,297.327411017952));
#2781=CARTESIAN_POINT('Ctrl Pts',(-2.80916732135543,1.58263419469439,297.333591752682));
#2782=CARTESIAN_POINT('Ctrl Pts',(-2.8569801844651,1.4945822491352,297.339772487412));
#2783=CARTESIAN_POINT('Ctrl Pts',(-2.90055185139118,1.40460546769945,297.345953222142));
#2784=CARTESIAN_POINT('Ctrl Pts',(-2.94419234272329,1.31448656182883,297.352143719762));
#2785=CARTESIAN_POINT('Ctrl Pts',(-2.98357808941882,1.22243714456876,297.358334217382));
#2786=CARTESIAN_POINT('Ctrl Pts',(-3.01856020756448,1.12889850553906,297.364524715002));
#2787=CARTESIAN_POINT('Ctrl Pts',(-3.03942608990356,1.07310525059589,297.368217178517));
#2788=CARTESIAN_POINT('Ctrl Pts',(-3.0587262063523,1.01678246065064,297.371909642033));
#2789=CARTESIAN_POINT('Ctrl Pts',(-3.07643756647016,0.960025761170579,297.375602105549));
#2790=CARTESIAN_POINT('Ctrl Pts',(-3.10606820094873,0.865073312272688,297.381779498817));
#2791=CARTESIAN_POINT('Ctrl Pts',(-3.13134962751106,0.768584728667232,297.387956892085));
#2792=CARTESIAN_POINT('Ctrl Pts',(-3.15212371614888,0.670994516066822,297.394134285353));
#2793=CARTESIAN_POINT('Ctrl Pts',(-3.17287014539651,0.573534238686073,297.400303453812));
#2794=CARTESIAN_POINT('Ctrl Pts',(-3.18912107616278,0.474975668252509,297.40647262227));
#2795=CARTESIAN_POINT('Ctrl Pts',(-3.2007678817287,0.37576925072976,297.412641790728));
#2796=CARTESIAN_POINT('Ctrl Pts',(-3.21240260373906,0.276665759820667,297.418804558677));
#2797=CARTESIAN_POINT('Ctrl Pts',(-3.21944264763299,0.176916186463936,297.424967326625));
#2798=CARTESIAN_POINT('Ctrl Pts',(-3.22183045528502,0.0769810359627175,
297.431130094574));
#2799=CARTESIAN_POINT('Ctrl Pts',(-3.22421656964183,-0.022883246303877,
297.437288492244));
#2800=CARTESIAN_POINT('Ctrl Pts',(-3.22195699700505,-0.122932411931123,
297.443446889914));
#2801=CARTESIAN_POINT('Ctrl Pts',(-3.21504610200097,-0.222701873607629,
297.449605287583));
#2802=CARTESIAN_POINT('Ctrl Pts',(-3.20813771679354,-0.322435102486507,
297.455761448737));
#2803=CARTESIAN_POINT('Ctrl Pts',(-3.19658139593122,-0.421888397275395,
297.461917609891));
#2804=CARTESIAN_POINT('Ctrl Pts',(-3.18042357849842,-0.520599100874478,
297.468073771045));
#2805=CARTESIAN_POINT('Ctrl Pts',(-3.16426732873914,-0.619300227303995,
297.474229334912));
#2806=CARTESIAN_POINT('Ctrl Pts',(-3.14351054030028,-0.717258478044924,
297.480384898779));
#2807=CARTESIAN_POINT('Ctrl Pts',(-3.1182511545876,-0.814019225456698,297.486540462647));
#2808=CARTESIAN_POINT('Ctrl Pts',(-3.09298749710563,-0.910796336670578,
297.492697067519));
#2809=CARTESIAN_POINT('Ctrl Pts',(-3.06321983936119,-1.0063751228674,297.498853672391));
#2810=CARTESIAN_POINT('Ctrl Pts',(-3.02909632157031,-1.10031497179181,297.505010277263));
#2811=CARTESIAN_POINT('Ctrl Pts',(-2.99493701929128,-1.19435333310969,297.511173338415));
#2812=CARTESIAN_POINT('Ctrl Pts',(-2.95641288494598,-1.28674891743634,297.517336399566));
#2813=CARTESIAN_POINT('Ctrl Pts',(-2.91372061764584,-1.37708014465591,297.523499460717));
#2814=CARTESIAN_POINT('Ctrl Pts',(-2.87100408196638,-1.46746272057691,297.529666025255));
#2815=CARTESIAN_POINT('Ctrl Pts',(-2.82411489797059,-1.55577821966582,297.535832589793));
#2816=CARTESIAN_POINT('Ctrl Pts',(-2.77329526067888,-1.64163057951418,297.54199915433));
#2817=CARTESIAN_POINT('Ctrl Pts',(-2.72239482155023,-1.72761944227266,297.548175523537));
#2818=CARTESIAN_POINT('Ctrl Pts',(-2.66755168691305,-1.81113698255652,297.554351892744));
#2819=CARTESIAN_POINT('Ctrl Pts',(-2.60905081857773,-1.89181695430052,297.560528261951));
#2820=CARTESIAN_POINT('Ctrl Pts',(-2.57277371178145,-1.94184759546128,297.564358304337));
#2821=CARTESIAN_POINT('Ctrl Pts',(-2.53509087092948,-1.99078772839539,297.568188346723));
#2822=CARTESIAN_POINT('Ctrl Pts',(-2.49607753242807,-2.03855696869325,297.572018389109));
#2823=CARTESIAN_POINT('Ctrl Pts',(-2.43309809797871,-2.1156711007721,297.578201246374));
#2824=CARTESIAN_POINT('Ctrl Pts',(-2.36643510744065,-2.18999455866235,297.584384103639));
#2825=CARTESIAN_POINT('Ctrl Pts',(-2.2963650479526,-2.26115570650092,297.590566960904));
#2826=CARTESIAN_POINT('Ctrl Pts',(-2.22640572126366,-2.33220439727657,297.596740047304));
#2827=CARTESIAN_POINT('Ctrl Pts',(-2.15305033958826,-2.40010041536909,297.602913133704));
#2828=CARTESIAN_POINT('Ctrl Pts',(-2.07661568444226,-2.46450499322448,297.609086220104));
#2829=CARTESIAN_POINT('Ctrl Pts',(-2.00025084138479,-2.52885074674054,297.615253668275));
#2830=CARTESIAN_POINT('Ctrl Pts',(-1.92081264186164,-2.58971111871789,297.621421116447));
#2831=CARTESIAN_POINT('Ctrl Pts',(-1.83865445309451,-2.64678434418366,297.627588564618));
#2832=CARTESIAN_POINT('Ctrl Pts',(-1.75655585229805,-2.70381617538629,297.633751539642));
#2833=CARTESIAN_POINT('Ctrl Pts',(-1.67174153991997,-2.75706607659332,297.639914514665));
#2834=CARTESIAN_POINT('Ctrl Pts',(-1.58459681948458,-2.80627341543538,297.646077489689));
#2835=CARTESIAN_POINT('Ctrl Pts',(-1.54860681629195,-2.82659561364978,297.648622744177));
#2836=CARTESIAN_POINT('Ctrl Pts',(-1.51221969163722,-2.84622880610641,297.651167998664));
#2837=CARTESIAN_POINT('Ctrl Pts',(-1.47546400239267,-2.86515680899727,297.653713253152));
#2838=CARTESIAN_POINT('',(-1.87158653173916,2.62360084935048,297.));
#2839=CARTESIAN_POINT('Origin',(0.,0.,297.));
#2840=CARTESIAN_POINT('Ctrl Pts',(-1.87158653173917,2.62360084935048,297.));
#2841=CARTESIAN_POINT('Ctrl Pts',(-1.89151501090213,2.60938455832866,297.001511146392));
#2842=CARTESIAN_POINT('Ctrl Pts',(-1.91128147124222,2.5949412363802,297.00300977116));
#2843=CARTESIAN_POINT('Ctrl Pts',(-1.95983501508414,2.55860742914849,297.006694908871));
#2844=CARTESIAN_POINT('Ctrl Pts',(-1.98842232314421,2.53645463522962,297.008868175637));
#2845=CARTESIAN_POINT('Ctrl Pts',(-2.13255247496678,2.42083104011892,297.01987385646));
#2846=CARTESIAN_POINT('Ctrl Pts',(-2.24191063438775,2.31992370603537,297.028391387703));
#2847=CARTESIAN_POINT('Ctrl Pts',(-2.46530621998206,2.08318620708576,297.047026520952));
#2848=CARTESIAN_POINT('Ctrl Pts',(-2.57589028177142,1.94478371461386,297.057118274445));
#2849=CARTESIAN_POINT('Ctrl Pts',(-2.70940464418189,1.74618011739376,297.071255356244));
#2850=CARTESIAN_POINT('Ctrl Pts',(-2.74273483708399,1.69334683074426,297.074984204102));
#2851=CARTESIAN_POINT('Ctrl Pts',(-2.7950495198796,1.60481962890104,297.081204455471));
#2852=CARTESIAN_POINT('Ctrl Pts',(-2.81493561634823,1.56967676057289,297.083666710306));
#2853=CARTESIAN_POINT('Ctrl Pts',(-2.8532321465274,1.49892952774936,297.088615648114));
#2854=CARTESIAN_POINT('Ctrl Pts',(-2.87164905468074,1.46333690847566,297.091101568197));
#2855=CARTESIAN_POINT('Ctrl Pts',(-2.91608813159483,1.37338236282152,297.097380141935));
#2856=CARTESIAN_POINT('Ctrl Pts',(-2.94125721501756,1.31861835794363,297.101198954259));
#2857=CARTESIAN_POINT('Ctrl Pts',(-3.06310458212016,1.03262491785649,297.121145009664));
#2858=CARTESIAN_POINT('Ctrl Pts',(-3.13409080569824,0.791428840294966,297.13806703326));
#2859=CARTESIAN_POINT('Ctrl Pts',(-3.19560910512955,0.432550735117186,297.162772691734));
#2860=CARTESIAN_POINT('Ctrl Pts',(-3.2088682612389,0.319663245654916,297.170462687525));
#2861=CARTESIAN_POINT('Ctrl Pts',(-3.21914654228964,0.159434016087073,297.181108231019));
#2862=CARTESIAN_POINT('Ctrl Pts',(-3.22112839309526,0.112498732676699,297.184193686169));
#2863=CARTESIAN_POINT('Ctrl Pts',(-3.22283301721058,0.0286891419506858,
297.189627765798));
#2864=CARTESIAN_POINT('Ctrl Pts',(-3.22295039765794,-0.00816845506468047,
297.191991529349));
#2865=CARTESIAN_POINT('Ctrl Pts',(-3.22213315783248,-0.0666625260269022,
297.195693911339));
#2866=CARTESIAN_POINT('Ctrl Pts',(-3.22161280522507,-0.0883004785492859,
297.197052839046));
#2867=CARTESIAN_POINT('Ctrl Pts',(-3.22016204112837,-0.130806011876565,
297.199699403599));
#2868=CARTESIAN_POINT('Ctrl Pts',(-3.2192466890242,-0.15167255601355,297.200987579638));
#2869=CARTESIAN_POINT('Ctrl Pts',(-3.21629995036034,-0.206637096286946,
297.20435494168));
#2870=CARTESIAN_POINT('Ctrl Pts',(-3.21392914815483,-0.240715394021917,
297.206416577875));
#2871=CARTESIAN_POINT('Ctrl Pts',(-3.19355424788907,-0.47883694661062,297.220679927958));
#2872=CARTESIAN_POINT('Ctrl Pts',(-3.15667236462029,-0.68081800582869,297.232069265853));
#2873=CARTESIAN_POINT('Ctrl Pts',(-3.05209968839318,-1.05016165625582,297.253659071756));
#2874=CARTESIAN_POINT('Ctrl Pts',(-2.9890851907885,-1.2179954617432,297.263791240634));
#2875=CARTESIAN_POINT('Ctrl Pts',(-2.89116624536072,-1.42469347743832,297.277321614191));
#2876=CARTESIAN_POINT('Ctrl Pts',(-2.86882461384046,-1.46916258475178,297.280296856216));
#2877=CARTESIAN_POINT('Ctrl Pts',(-2.82908961162629,-1.5438865742787,297.285417905799));
#2878=CARTESIAN_POINT('Ctrl Pts',(-2.81221773925494,-1.5744094204346,297.287545228085));
#2879=CARTESIAN_POINT('Ctrl Pts',(-2.77679274541169,-1.6361098551466,297.291921949513));
#2880=CARTESIAN_POINT('Ctrl Pts',(-2.75820190641163,-1.66725987159154,297.294172499382));
#2881=CARTESIAN_POINT('Ctrl Pts',(-2.70887846405452,-1.74682070859336,297.300030720848));
#2882=CARTESIAN_POINT('Ctrl Pts',(-2.67737365654439,-1.7947352844465,297.303666606203));
#2883=CARTESIAN_POINT('Ctrl Pts',(-2.51535548869813,-2.02737671830831,297.321873988285));
#2884=CARTESIAN_POINT('Ctrl Pts',(-2.36694320299785,-2.19882201149093,297.33713143598));
#2885=CARTESIAN_POINT('Ctrl Pts',(-2.07642187633599,-2.47064582761142,297.364161641344));
#2886=CARTESIAN_POINT('Ctrl Pts',(-1.94180921729375,-2.57779094123865,297.375828218173));
#2887=CARTESIAN_POINT('Ctrl Pts',(-1.77165654763903,-2.69229638299389,297.389088817439));
#2888=CARTESIAN_POINT('Ctrl Pts',(-1.74373830172358,-2.71046189452414,297.391219825866));
#2889=CARTESIAN_POINT('Ctrl Pts',(-1.69839475250396,-2.73897483142018,297.394603283233));
#2890=CARTESIAN_POINT('Ctrl Pts',(-1.68114546687041,-2.74959594696396,297.395872611772));
#2891=CARTESIAN_POINT('Ctrl Pts',(-1.64565612078635,-2.77098937504568,297.39844683352));
#2892=CARTESIAN_POINT('Ctrl Pts',(-1.62740842460557,-2.7817455063204,297.399750915196));
#2893=CARTESIAN_POINT('Ctrl Pts',(-1.57842496984379,-2.80997187616802,297.403203392058));
#2894=CARTESIAN_POINT('Ctrl Pts',(-1.54750474949298,-2.82711807487197,297.405332765564));
#2895=CARTESIAN_POINT('Ctrl Pts',(-1.50274205757047,-2.85098582998335,297.408353435895));
#2896=CARTESIAN_POINT('Ctrl Pts',(-1.48912726939844,-2.85812066414376,297.409264091));
#2897=CARTESIAN_POINT('Ctrl Pts',(-1.47546398584926,-2.86515681751659,297.410170442659));
#2898=CARTESIAN_POINT('Origin',(0.,0.,294.689226550727));
#2899=CARTESIAN_POINT('',(-1.47546409036591,-2.86515676369386,298.903152516993));
#2900=CARTESIAN_POINT('',(-1.47546399981363,-2.86515681032539,298.654589343883));
#2901=CARTESIAN_POINT('',(-1.47546400239267,-2.86515680899727,294.689226550727));
#2902=CARTESIAN_POINT('',(3.22274999369119,-0.000201651753011577,298.060773449234));
#2903=CARTESIAN_POINT('Ctrl Pts',(-1.47546409036594,-2.86515676369385,298.903152516993));
#2904=CARTESIAN_POINT('Ctrl Pts',(-1.6591960385397,-2.77054068710826,298.891552718834));
#2905=CARTESIAN_POINT('Ctrl Pts',(-1.83345625504359,-2.65844361410806,298.879965681433));
#2906=CARTESIAN_POINT('Ctrl Pts',(-2.03848911916688,-2.49672422759705,298.864567628018));
#2907=CARTESIAN_POINT('Ctrl Pts',(-2.08029032183093,-2.46200354033995,298.861327433074));
#2908=CARTESIAN_POINT('Ctrl Pts',(-2.14590885635884,-2.404635232992,298.856062741298));
#2909=CARTESIAN_POINT('Ctrl Pts',(-2.17029311842409,-2.3826504324519,298.854064920298));
#2910=CARTESIAN_POINT('Ctrl Pts',(-2.22076152090531,-2.33573064346003,298.849839082774));
#2911=CARTESIAN_POINT('Ctrl Pts',(-2.24677114267321,-2.31072253620592,298.847608164488));
#2912=CARTESIAN_POINT('Ctrl Pts',(-2.30930897980404,-2.24853851159302,298.842109267261));
#2913=CARTESIAN_POINT('Ctrl Pts',(-2.3453648036758,-2.21090407871771,298.83882178845));
#2914=CARTESIAN_POINT('Ctrl Pts',(-2.51658583690561,-2.02328323331635,298.822616507258));
#2915=CARTESIAN_POINT('Ctrl Pts',(-2.6383466108852,-1.86171539963794,298.809175177368));
#2916=CARTESIAN_POINT('Ctrl Pts',(-2.84071143788486,-1.53309064159345,298.783168906886));
#2917=CARTESIAN_POINT('Ctrl Pts',(-2.92363824819888,-1.36834082840619,298.7706881872));
#2918=CARTESIAN_POINT('Ctrl Pts',(-3.00578395655033,-1.16307666829401,298.756382966809));
#2919=CARTESIAN_POINT('Ctrl Pts',(-3.0189299383629,-1.12851531661196,298.75401545357));
#2920=CARTESIAN_POINT('Ctrl Pts',(-3.03879817190377,-1.07344695303929,298.750316131406));
#2921=CARTESIAN_POINT('Ctrl Pts',(-3.04591391774224,-1.05308649083907,298.748963961046));
#2922=CARTESIAN_POINT('Ctrl Pts',(-3.0595761224216,-1.012697105867,298.746314456983));
#2923=CARTESIAN_POINT('Ctrl Pts',(-3.06613155932879,-0.992672544564584,
298.745016737267));
#2924=CARTESIAN_POINT('Ctrl Pts',(-3.08291771229299,-0.939643440628762,
298.741618383366));
#2925=CARTESIAN_POINT('Ctrl Pts',(-3.09281515472522,-0.906535188865807,
298.739535501352));
#2926=CARTESIAN_POINT('Ctrl Pts',(-3.11392929785717,-0.831530161019412,
298.734890812584));
#2927=CARTESIAN_POINT('Ctrl Pts',(-3.12483674935978,-0.789552846483335,
298.732342774009));
#2928=CARTESIAN_POINT('Ctrl Pts',(-3.15828145695989,-0.649266082201744,
298.723959497458));
#2929=CARTESIAN_POINT('Ctrl Pts',(-3.17705246238441,-0.550116424821424,
298.718247236005));
#2930=CARTESIAN_POINT('Ctrl Pts',(-3.22499356732628,-0.210330398377229,
298.698932430009));
#2931=CARTESIAN_POINT('Ctrl Pts',(-3.23167902450801,0.0326145108600474,
298.685497356927));
#2932=CARTESIAN_POINT('Ctrl Pts',(-3.20649373452886,0.327758383857938,298.668024653567));
#2933=CARTESIAN_POINT('Ctrl Pts',(-3.2005585338958,0.381381969750893,298.664806732028));
#2934=CARTESIAN_POINT('Ctrl Pts',(-3.18885961360891,0.46729601691632,298.659568379224));
#2935=CARTESIAN_POINT('Ctrl Pts',(-3.1839438446911,0.499692582311363,298.657574098447));
#2936=CARTESIAN_POINT('Ctrl Pts',(-3.17256922501014,0.567651427338976,298.653347858176));
#2937=CARTESIAN_POINT('Ctrl Pts',(-3.1660044147582,0.603191106258999,298.651112875841));
#2938=CARTESIAN_POINT('Ctrl Pts',(-3.14844664871458,0.69003923113951,298.645587125001));
#2939=CARTESIAN_POINT('Ctrl Pts',(-3.13679592483552,0.741202577938277,298.642276401362));
#2940=CARTESIAN_POINT('Ctrl Pts',(-3.07527219724289,0.983854585014435,298.626300206029));
#2941=CARTESIAN_POINT('Ctrl Pts',(-3.00908909751798,1.17073940105393,298.613135594628));
#2942=CARTESIAN_POINT('Ctrl Pts',(-2.8476123523373,1.5206586346405,298.587172357915));
#2943=CARTESIAN_POINT('Ctrl Pts',(-2.75429821604088,1.68379009583437,298.574447194288));
#2944=CARTESIAN_POINT('Ctrl Pts',(-2.62630800401366,1.86814911927084,298.559927696015));
#2945=CARTESIAN_POINT('Ctrl Pts',(-2.60477938358137,1.89805149743848,298.557568832788));
#2946=CARTESIAN_POINT('Ctrl Pts',(-2.56985873263698,1.94484127813371,298.553879806655));
#2947=CARTESIAN_POINT('Ctrl Pts',(-2.55680258421338,1.96197403370382,298.552529460067));
#2948=CARTESIAN_POINT('Ctrl Pts',(-2.53062283313602,1.99562284741262,298.549880372227));
#2949=CARTESIAN_POINT('Ctrl Pts',(-2.51750700065251,2.01214338918097,298.54858129126));
#2950=CARTESIAN_POINT('Ctrl Pts',(-2.48240929964527,2.05547156835581,298.545174797424));
#2951=CARTESIAN_POINT('Ctrl Pts',(-2.46015481709589,2.08205614496051,298.543085291257));
#2952=CARTESIAN_POINT('Ctrl Pts',(-2.40898051929473,2.14122105581336,298.538423026225));
#2953=CARTESIAN_POINT('Ctrl Pts',(-2.37982011345836,2.17358489831474,298.535864193234));
#2954=CARTESIAN_POINT('Ctrl Pts',(-2.28046718034941,2.27945499922921,298.527426252839));
#2955=CARTESIAN_POINT('Ctrl Pts',(-2.20745263262055,2.35023419787734,298.521671815143));
#2956=CARTESIAN_POINT('Ctrl Pts',(-1.9507171707951,2.57657108956049,298.502410249197));
#2957=CARTESIAN_POINT('Ctrl Pts',(-1.75298689405621,2.71496659631791,298.489062451772));
#2958=CARTESIAN_POINT('Ctrl Pts',(-1.49412873871142,2.85598174572173,298.471678239932));
#2959=CARTESIAN_POINT('Ctrl Pts',(-1.44591171104451,2.88069284127834,298.468447183325));
#2960=CARTESIAN_POINT('Ctrl Pts',(-1.36753443702595,2.91839738624888,298.463193249873));
#2961=CARTESIAN_POINT('Ctrl Pts',(-1.33775757184079,2.93216614456803,298.461196831334));
#2962=CARTESIAN_POINT('Ctrl Pts',(-1.27477687403119,2.96012924239569,298.456970696247));
#2963=CARTESIAN_POINT('Ctrl Pts',(-1.24153443779829,2.97422482085654,298.454738027793));
#2964=CARTESIAN_POINT('Ctrl Pts',(-1.1596124682817,3.00734895671664,298.449227872593));
#2965=CARTESIAN_POINT('Ctrl Pts',(-1.11069473316829,3.02575701848861,298.445930698259));
#2966=CARTESIAN_POINT('Ctrl Pts',(-1.00373266373073,3.06306420681997,298.438702423404));
#2967=CARTESIAN_POINT('Ctrl Pts',(-0.94555598457028,3.08151987491369,298.434759158993));
#2968=CARTESIAN_POINT('Ctrl Pts',(-0.764296860510881,3.13340538089995,298.422440913458));
#2969=CARTESIAN_POINT('Ctrl Pts',(-0.639734933850608,3.1611886328633,298.413925238229));
#2970=CARTESIAN_POINT('Ctrl Pts',(-0.317205756116933,3.21328203832322,298.391933079726));
#2971=CARTESIAN_POINT('Ctrl Pts',(-0.118015487143215,3.22674490844994,298.378388921139));
#2972=CARTESIAN_POINT('Ctrl Pts',(0.116922403576108,3.22082707674956,298.363201765964));
#2973=CARTESIAN_POINT('Ctrl Pts',(0.152677183535147,3.21933033795137,298.360912942984));
#2974=CARTESIAN_POINT('Ctrl Pts',(0.209686893482735,3.21599185352485,298.357306970387));
#2975=CARTESIAN_POINT('Ctrl Pts',(0.230960350489543,3.21453411412291,298.355971068119));
#2976=CARTESIAN_POINT('Ctrl Pts',(0.27345431084657,3.2111982254573,298.353324035055));
#2977=CARTESIAN_POINT('Ctrl Pts',(0.294673798092116,3.20932060006801,298.35201294946));
#2978=CARTESIAN_POINT('Ctrl Pts',(0.351372827070678,3.20373642872578,298.348534700757));
#2979=CARTESIAN_POINT('Ctrl Pts',(0.386813015016976,3.19965090167405,298.3463868294));
#2980=CARTESIAN_POINT('Ctrl Pts',(0.467055241463996,3.18904781164447,298.341568726853));
#2981=CARTESIAN_POINT('Ctrl Pts',(0.511802945558486,3.18217294500449,298.338913868008));
#2982=CARTESIAN_POINT('Ctrl Pts',(0.663536742366492,3.15557745095116,298.329976816981));
#2983=CARTESIAN_POINT('Ctrl Pts',(0.769667143674456,3.13138389696102,298.323835245966));
#2984=CARTESIAN_POINT('Ctrl Pts',(1.09182626101457,3.04057149360314,298.305021351661));
#2985=CARTESIAN_POINT('Ctrl Pts',(1.30220933664901,2.95658604124506,298.292444842921));
#2986=CARTESIAN_POINT('Ctrl Pts',(1.55160365214098,2.82520396911323,298.275847268083));
#2987=CARTESIAN_POINT('Ctrl Pts',(1.60044111024342,2.79782756224527,298.27251290614));
#2988=CARTESIAN_POINT('Ctrl Pts',(1.68013606286744,2.75038407921992,298.266915308918));
#2989=CARTESIAN_POINT('Ctrl Pts',(1.7114079881714,2.73103502392164,298.264677522831));
#2990=CARTESIAN_POINT('Ctrl Pts',(1.77301028584244,2.69144592487489,298.260182490146));
#2991=CARTESIAN_POINT('Ctrl Pts',(1.80334184377295,2.67121782427452,298.257925906087));
#2992=CARTESIAN_POINT('Ctrl Pts',(1.87793243713751,2.61962391437302,298.252264443833));
#2993=CARTESIAN_POINT('Ctrl Pts',(1.92175370357352,2.58764793539101,298.248837315161));
#2994=CARTESIAN_POINT('Ctrl Pts',(2.11960578197402,2.43547869585365,298.232881974063));
#2995=CARTESIAN_POINT('Ctrl Pts',(2.2632940852352,2.30255621012592,298.21987474582));
#2996=CARTESIAN_POINT('Ctrl Pts',(2.51863696368645,2.01921315438659,298.194175827212));
#2997=CARTESIAN_POINT('Ctrl Pts',(2.63102481851755,1.87042006772774,298.181553379709));
#2998=CARTESIAN_POINT('Ctrl Pts',(2.7495606857906,1.6814861753241,298.167123046619));
#2999=CARTESIAN_POINT('Ctrl Pts',(2.76863783192965,1.64988622025523,298.164759837543));
#3000=CARTESIAN_POINT('Ctrl Pts',(2.79798973231079,1.59932347695914,298.161065601027));
#3001=CARTESIAN_POINT('Ctrl Pts',(2.80862375159028,1.58057420227658,298.159714301926));
#3002=CARTESIAN_POINT('Ctrl Pts',(2.82927960006955,1.54328819588219,298.157065651632));
#3003=CARTESIAN_POINT('Ctrl Pts',(2.83930923909406,1.52475722600699,298.155767930978));
#3004=CARTESIAN_POINT('Ctrl Pts',(2.86532023960482,1.47555199424044,298.152367591886));
#3005=CARTESIAN_POINT('Ctrl Pts',(2.88099128038311,1.4447156190346,298.150282785567));
#3006=CARTESIAN_POINT('Ctrl Pts',(2.91521223602377,1.3746057788721,298.145632733273));
#3007=CARTESIAN_POINT('Ctrl Pts',(2.93347100913079,1.3351972120616,298.143081316996));
#3008=CARTESIAN_POINT('Ctrl Pts',(2.99157234195457,1.2028451150518,298.134680033881));
#3009=CARTESIAN_POINT('Ctrl Pts',(3.02783877354474,1.10839345233708,298.128953805258));
#3010=CARTESIAN_POINT('Ctrl Pts',(3.13288996364184,0.790911305705543,298.110133298698));
#3011=CARTESIAN_POINT('Ctrl Pts',(3.1819049131835,0.562150509798829,298.097193790661));
#3012=CARTESIAN_POINT('Ctrl Pts',(3.21164346314507,0.273348893061976,298.080131172405));
#3013=CARTESIAN_POINT('Ctrl Pts',(3.21597939596838,0.216447001981912,298.07673857764));
#3014=CARTESIAN_POINT('Ctrl Pts',(3.22027761091772,0.129686066079792,298.071503986356));
#3015=CARTESIAN_POINT('Ctrl Pts',(3.22133946752476,0.0998915044040692,298.06969537231));
#3016=CARTESIAN_POINT('Ctrl Pts',(3.22249863186971,0.0466034311486563,298.066439097593));
#3017=CARTESIAN_POINT('Ctrl Pts',(3.22275269597726,0.0231153400034857,298.064996338945));
#3018=CARTESIAN_POINT('Ctrl Pts',(3.22274997842995,-0.000372866926442411,
298.063545698078));
#3019=CARTESIAN_POINT('Ctrl Pts',(-1.47546400239267,-2.86515680899727,297.653713253152));
#3020=CARTESIAN_POINT('Ctrl Pts',(-1.3864988722017,-2.91097100201203,297.659873902062));
#3021=CARTESIAN_POINT('Ctrl Pts',(-1.295372951794,-2.9526505390965,297.666034550972));
#3022=CARTESIAN_POINT('Ctrl Pts',(-1.20250825355637,-2.98999857234562,297.672195199882));
#3023=CARTESIAN_POINT('Ctrl Pts',(-1.10964207451035,-3.02734720114161,297.678355947028));
#3024=CARTESIAN_POINT('Ctrl Pts',(-1.01503746431377,-3.06036402808895,297.684516694175));
#3025=CARTESIAN_POINT('Ctrl Pts',(-0.919135749817075,-3.0889006192994,297.690677441322));
#3026=CARTESIAN_POINT('Ctrl Pts',(-0.818267954305444,-3.11891492156627,
297.697157210601));
#3027=CARTESIAN_POINT('Ctrl Pts',(-0.715965614330064,-3.14397235708149,
297.70363697988));
#3028=CARTESIAN_POINT('Ctrl Pts',(-0.612757774231671,-3.16396040945816,
297.710116749159));
#3029=CARTESIAN_POINT('Ctrl Pts',(-0.514492453227045,-3.18299125421935,
297.71628620884));
#3030=CARTESIAN_POINT('Ctrl Pts',(-0.415406804278566,-3.19742702253057,
297.722455668521));
#3031=CARTESIAN_POINT('Ctrl Pts',(-0.315964162543643,-3.2072237543533,297.728625128201));
#3032=CARTESIAN_POINT('Ctrl Pts',(-0.216454009223977,-3.21702713717484,
297.734798776327));
#3033=CARTESIAN_POINT('Ctrl Pts',(-0.116586811851768,-3.22218519139546,
297.740972424452));
#3034=CARTESIAN_POINT('Ctrl Pts',(-0.0168268071893892,-3.22270607115508,
297.747146072578));
#3035=CARTESIAN_POINT('Ctrl Pts',(0.0830782578465212,-3.22322770832257,
297.753328697765));
#3036=CARTESIAN_POINT('Ctrl Pts',(0.182875388517365,-3.2190987360934,297.759511322952));
#3037=CARTESIAN_POINT('Ctrl Pts',(0.282104855435379,-3.21037916966825,297.765693948139));
#3038=CARTESIAN_POINT('Ctrl Pts',(0.296767485300708,-3.20909072401748,297.766607522983));
#3039=CARTESIAN_POINT('Ctrl Pts',(0.311417738880869,-3.20770213618914,297.767521097826));
#3040=CARTESIAN_POINT('Ctrl Pts',(0.326054153801449,-3.20621369395255,297.76843467267));
#3041=CARTESIAN_POINT('Ctrl Pts',(0.425105640416448,-3.19614070701722,297.77461726225));
#3042=CARTESIAN_POINT('Ctrl Pts',(0.523857142175329,-3.18145634053772,297.780799851831));
#3043=CARTESIAN_POINT('Ctrl Pts',(0.621846278658205,-3.16218670672985,297.786982441412));
#3044=CARTESIAN_POINT('Ctrl Pts',(0.71970621202586,-3.14294248080704,297.793156878968));
#3045=CARTESIAN_POINT('Ctrl Pts',(0.816805357319707,-3.11912508864679,297.799331316524));
#3046=CARTESIAN_POINT('Ctrl Pts',(0.912686224488411,-3.09081242040488,297.80550575408));
#3047=CARTESIAN_POINT('Ctrl Pts',(1.00846870967552,-3.06252880338548,297.811673856135));
#3048=CARTESIAN_POINT('Ctrl Pts',(1.1030349894859,-3.0297592034546,297.817841958189));
#3049=CARTESIAN_POINT('Ctrl Pts',(1.19593847430688,-2.99263240779293,297.824010060244));
#3050=CARTESIAN_POINT('Ctrl Pts',(1.28877726195373,-2.955531466907,297.830173866886));
#3051=CARTESIAN_POINT('Ctrl Pts',(1.37995515640695,-2.91407952363585,297.836337673528));
#3052=CARTESIAN_POINT('Ctrl Pts',(1.46904228340674,-2.86845469409281,297.84250148017));
#3053=CARTESIAN_POINT('Ctrl Pts',(1.55809772307698,-2.82284609280921,297.848663094413));
#3054=CARTESIAN_POINT('Ctrl Pts',(1.64506348851173,-2.77306775193101,297.854824708656));
#3055=CARTESIAN_POINT('Ctrl Pts',(1.72953200026501,-2.71934488849048,297.860986322898));
#3056=CARTESIAN_POINT('Ctrl Pts',(1.81399283656353,-2.66562690672005,297.86714737725));
#3057=CARTESIAN_POINT('Ctrl Pts',(1.89595650546268,-2.60796534743763,297.873308431601));
#3058=CARTESIAN_POINT('Ctrl Pts',(1.97504309248858,-2.54662960504922,297.879469485952));
#3059=CARTESIAN_POINT('Ctrl Pts',(2.05414343654389,-2.48528319337233,297.885631612012));
#3060=CARTESIAN_POINT('Ctrl Pts',(2.13036536272108,-2.42026159413796,297.891793738073));
#3061=CARTESIAN_POINT('Ctrl Pts',(2.20336160092606,-2.35187483044157,297.897955864133));
#3062=CARTESIAN_POINT('Ctrl Pts',(2.27643448021811,-2.28341626529294,297.904124460007));
#3063=CARTESIAN_POINT('Ctrl Pts',(2.34627459326325,-2.21158577753458,297.91029305588));
#3064=CARTESIAN_POINT('Ctrl Pts',(2.41257127322473,-2.13673054316889,297.916461651754));
#3065=CARTESIAN_POINT('Ctrl Pts',(2.47890577301725,-2.06183260662991,297.922633766586));
#3066=CARTESIAN_POINT('Ctrl Pts',(2.54169254259044,-1.98390682376247,297.928805881418));
#3067=CARTESIAN_POINT('Ctrl Pts',(2.60066226735119,-1.90333216588061,297.93497799625));
#3068=CARTESIAN_POINT('Ctrl Pts',(2.65972538334018,-1.82262990071729,297.941159885952));
#3069=CARTESIAN_POINT('Ctrl Pts',(2.71495914327061,-1.73927074331159,297.947341775654));
#3070=CARTESIAN_POINT('Ctrl Pts',(2.76613846154025,-1.65366126340546,297.953523665355));
#3071=CARTESIAN_POINT('Ctrl Pts',(2.79739767475446,-1.60137285715033,297.95729942898));
#3072=CARTESIAN_POINT('Ctrl Pts',(2.82714528212604,-1.5482454479238,297.961075192605));
#3073=CARTESIAN_POINT('Ctrl Pts',(2.8553387868184,-1.49437544646265,297.964850956229));
#3074=CARTESIAN_POINT('Ctrl Pts',(2.90406371299427,-1.40127556856774,297.971376352979));
#3075=CARTESIAN_POINT('Ctrl Pts',(2.94829409842913,-1.3056709537505,297.977901749728));
#3076=CARTESIAN_POINT('Ctrl Pts',(2.98778066801885,-1.20800837841169,297.984427146477));
#3077=CARTESIAN_POINT('Ctrl Pts',(3.02715878541849,-1.11061403909069,297.99093462084));
#3078=CARTESIAN_POINT('Ctrl Pts',(3.06181892203709,-1.01117333837293,297.997442095202));
#3079=CARTESIAN_POINT('Ctrl Pts',(3.09155861547018,-0.910155420580508,298.003949569565));
#3080=CARTESIAN_POINT('Ctrl Pts',(3.12124947881499,-0.809303365756907,298.010446359199));
#3081=CARTESIAN_POINT('Ctrl Pts',(3.14603588209779,-0.706879593528002,298.016943148833));
#3082=CARTESIAN_POINT('Ctrl Pts',(3.16576366259527,-0.603372186209608,298.023439938467));
#3083=CARTESIAN_POINT('Ctrl Pts',(3.18544680753346,-0.500098972039173,298.029922028635));
#3084=CARTESIAN_POINT('Ctrl Pts',(3.20009407460375,-0.39574736234028,298.036404118803));
#3085=CARTESIAN_POINT('Ctrl Pts',(3.20960157544718,-0.290818309923867,298.042886208972));
#3086=CARTESIAN_POINT('Ctrl Pts',(3.21834684883231,-0.194301542317404,298.048848622392));
#3087=CARTESIAN_POINT('Ctrl Pts',(3.22274391833166,-0.0972965918580311,
298.054811035813));
#3088=CARTESIAN_POINT('Ctrl Pts',(3.22274999369119,-0.000201651753011577,
298.060773449234));
#3089=CARTESIAN_POINT('Ctrl Pts',(-1.47546398584926,-2.86515681751659,297.410170442659));
#3090=CARTESIAN_POINT('Ctrl Pts',(-1.30851984510788,-2.95112770253292,297.421244654684));
#3091=CARTESIAN_POINT('Ctrl Pts',(-1.13433665046958,-3.02236604353812,297.431692562582));
#3092=CARTESIAN_POINT('Ctrl Pts',(-0.780905386326587,-3.13201051280962,
297.452458858485));
#3093=CARTESIAN_POINT('Ctrl Pts',(-0.602670515941956,-3.17113270153365,
297.462737748404));
#3094=CARTESIAN_POINT('Ctrl Pts',(-0.36765776902151,-3.20218057114698,297.476709960238));
#3095=CARTESIAN_POINT('Ctrl Pts',(-0.31304862087637,-3.20797953396451,297.479983403163));
#3096=CARTESIAN_POINT('Ctrl Pts',(-0.221646792429247,-3.21532951632577,
297.485520749532));
#3097=CARTESIAN_POINT('Ctrl Pts',(-0.184926767625853,-3.21765024839751,
297.487760958484));
#3098=CARTESIAN_POINT('Ctrl Pts',(-0.111162063892194,-3.22104540549316,
297.492296085474));
#3099=CARTESIAN_POINT('Ctrl Pts',(-0.0741225918464192,-3.22211051532846,
297.494590934589));
#3100=CARTESIAN_POINT('Ctrl Pts',(0.0193168099386926,-3.22318550257323,
297.50042767845));
#3101=CARTESIAN_POINT('Ctrl Pts',(0.0757121308366272,-3.22235395020963,
297.503994249201));
#3102=CARTESIAN_POINT('Ctrl Pts',(0.346136926652778,-3.21126382775852,297.521314803023));
#3103=CARTESIAN_POINT('Ctrl Pts',(0.558782943186501,-3.18115757680039,297.535642348083));
#3104=CARTESIAN_POINT('Ctrl Pts',(0.918787944819762,-3.09296315630843,297.56056829093));
#3105=CARTESIAN_POINT('Ctrl Pts',(1.06783819627523,-3.04472021935663,297.571082711752));
#3106=CARTESIAN_POINT('Ctrl Pts',(1.24620321896529,-2.9722709672623,297.583511944796));
#3107=CARTESIAN_POINT('Ctrl Pts',(1.27937469373764,-2.95814431683222,297.585816121074));
#3108=CARTESIAN_POINT('Ctrl Pts',(1.33202709175196,-2.93466995236105,297.589453917096));
#3109=CARTESIAN_POINT('Ctrl Pts',(1.35166232454172,-2.92567819884748,297.590806101317));
#3110=CARTESIAN_POINT('Ctrl Pts',(1.39077385678603,-2.90728965997207,297.593488464489));
#3111=CARTESIAN_POINT('Ctrl Pts',(1.41024883954537,-2.89789291529142,297.594818478245));
#3112=CARTESIAN_POINT('Ctrl Pts',(1.4625308623315,-2.8720147713772,297.598377589641));
#3113=CARTESIAN_POINT('Ctrl Pts',(1.49515427636117,-2.85516712469556,297.600586196206));
#3114=CARTESIAN_POINT('Ctrl Pts',(1.69584493983292,-2.74714133098956,297.614139594867));
#3115=CARTESIAN_POINT('Ctrl Pts',(1.85582581255376,-2.64170438231457,297.62481233139));
#3116=CARTESIAN_POINT('Ctrl Pts',(2.15696372202097,-2.40230149826316,297.646421192671));
#3117=CARTESIAN_POINT('Ctrl Pts',(2.29723812346219,-2.26853085700959,297.65732451832));
#3118=CARTESIAN_POINT('Ctrl Pts',(2.45954444485929,-2.08316157114292,297.671878148233));
#3119=CARTESIAN_POINT('Ctrl Pts',(2.49343526508803,-2.04247426454587,297.675040329777));
#3120=CARTESIAN_POINT('Ctrl Pts',(2.54890260773457,-1.97244453475001,297.680442309161));
#3121=CARTESIAN_POINT('Ctrl Pts',(2.57101250848631,-1.94353710118818,297.682660967959));
#3122=CARTESIAN_POINT('Ctrl Pts',(2.6122055521326,-1.88774630595666,297.68692520292));
#3123=CARTESIAN_POINT('Ctrl Pts',(2.6313750820318,-1.86093229718561,297.688967122066));
#3124=CARTESIAN_POINT('Ctrl Pts',(2.68097906322758,-1.78924790466129,297.694408671795));
#3125=CARTESIAN_POINT('Ctrl Pts',(2.71069724957047,-1.74389697792683,297.697833884215));
#3126=CARTESIAN_POINT('Ctrl Pts',(2.86656767873251,-1.49241625739937,297.716744568368));
#3127=CARTESIAN_POINT('Ctrl Pts',(2.97035410420162,-1.27337263094209,297.733001632057));
#3128=CARTESIAN_POINT('Ctrl Pts',(3.08147992048965,-0.949123700666557,297.756100300445));
#3129=CARTESIAN_POINT('Ctrl Pts',(3.10975813891146,-0.851915762275134,297.762897851485));
#3130=CARTESIAN_POINT('Ctrl Pts',(3.14358972444243,-0.711234154586975,297.772434921197));
#3131=CARTESIAN_POINT('Ctrl Pts',(3.15290514404828,-0.668730040466414,297.775277652372));
#3132=CARTESIAN_POINT('Ctrl Pts',(3.16809292173972,-0.592036316220455,297.7803234418));
#3133=CARTESIAN_POINT('Ctrl Pts',(3.17427939679768,-0.557916025582743,297.782538830892));
#3134=CARTESIAN_POINT('Ctrl Pts',(3.18335362306144,-0.502817295223105,297.786062140488));
#3135=CARTESIAN_POINT('Ctrl Pts',(3.18658727506148,-0.48189949120656,297.787387232875));
#3136=CARTESIAN_POINT('Ctrl Pts',(3.19269590812945,-0.439629922251756,297.790037676898));
#3137=CARTESIAN_POINT('Ctrl Pts',(3.1955633461254,-0.418278127082079,297.791362554702));
#3138=CARTESIAN_POINT('Ctrl Pts',(3.20277304752365,-0.360182199098518,297.794933427222));
#3139=CARTESIAN_POINT('Ctrl Pts',(3.20669714814887,-0.323388417396749,297.797158137567));
#3140=CARTESIAN_POINT('Ctrl Pts',(3.22623374077421,-0.104523251231982,297.810216194395));
#3141=CARTESIAN_POINT('Ctrl Pts',(3.22697258870022,0.078559510277362,297.820433044072));
#3142=CARTESIAN_POINT('Ctrl Pts',(3.19622541191419,0.457358281996847,297.841755255838));
#3143=CARTESIAN_POINT('Ctrl Pts',(3.16224788712159,0.652083027481734,297.852834716233));
#3144=CARTESIAN_POINT('Ctrl Pts',(3.09637610721237,0.895303617317299,297.867683841644));
#3145=CARTESIAN_POINT('Ctrl Pts',(3.08072445277333,0.947760463793996,297.870946278825));
#3146=CARTESIAN_POINT('Ctrl Pts',(3.05243690877041,1.03444439421292,297.876451838098));
#3147=CARTESIAN_POINT('Ctrl Pts',(3.04054179325477,1.06890211178701,297.878671016752));
#3148=CARTESIAN_POINT('Ctrl Pts',(3.01557161674428,1.13744342272423,297.883150610087));
#3149=CARTESIAN_POINT('Ctrl Pts',(3.00249683922268,1.17152135048366,297.885410743925));
#3150=CARTESIAN_POINT('Ctrl Pts',(2.96827952385552,1.25636700367486,297.891124136968));
#3151=CARTESIAN_POINT('Ctrl Pts',(2.94641169902695,1.30682779937892,297.894600848131));
#3152=CARTESIAN_POINT('Ctrl Pts',(2.82425710998779,1.57003236260474,297.913165277664));
#3153=CARTESIAN_POINT('Ctrl Pts',(2.70220846244861,1.77185395369853,297.928982119722));
#3154=CARTESIAN_POINT('Ctrl Pts',(2.4657745824985,2.08080916702227,297.955228105775));
#3155=CARTESIAN_POINT('Ctrl Pts',(2.36358216146528,2.19620096274597,297.965577804624));
#3156=CARTESIAN_POINT('Ctrl Pts',(2.23012892924665,2.32673883719612,297.977603991894));
#3157=CARTESIAN_POINT('Ctrl Pts',(2.20638459163562,2.34926709446119,297.979691748334));
#3158=CARTESIAN_POINT('Ctrl Pts',(2.16709529565289,2.38542292109452,297.983056780651));
#3159=CARTESIAN_POINT('Ctrl Pts',(2.15175551412132,2.39926922782389,297.984348995116));
#3160=CARTESIAN_POINT('Ctrl Pts',(2.11979539061685,2.42756461584974,297.986995296334));
#3161=CARTESIAN_POINT('Ctrl Pts',(2.10315832487625,2.44199254430847,297.98834801666));
#3162=CARTESIAN_POINT('Ctrl Pts',(2.05654892637634,2.4815832505092,297.992073599697));
#3163=CARTESIAN_POINT('Ctrl Pts',(2.02626329001173,2.5063731355181,297.994422131999));
#3164=CARTESIAN_POINT('Ctrl Pts',(1.83379911489679,2.65814247207678,298.008954389232));
#3165=CARTESIAN_POINT('Ctrl Pts',(1.66019443503162,2.76989411810704,298.020374493635));
#3166=CARTESIAN_POINT('Ctrl Pts',(1.33065379777891,2.93983428897944,298.041208192669));
#3167=CARTESIAN_POINT('Ctrl Pts',(1.17865120946816,3.00400392837138,298.050532628656));
#3168=CARTESIAN_POINT('Ctrl Pts',(0.967786311960895,3.07454480412374,298.063607085734));
#3169=CARTESIAN_POINT('Ctrl Pts',(0.912677883444726,3.09135157972572,298.067034476848));
#3170=CARTESIAN_POINT('Ctrl Pts',(0.821363761800754,3.11654574058412,298.072747166308));
#3171=CARTESIAN_POINT('Ctrl Pts',(0.785409786273584,3.12580022976907,298.075004817545));
#3172=CARTESIAN_POINT('Ctrl Pts',(0.714000112733848,3.14287115107033,298.079509081158));
#3173=CARTESIAN_POINT('Ctrl Pts',(0.678556272267247,3.15071364154695,298.081754497305));
#3174=CARTESIAN_POINT('Ctrl Pts',(0.590991197760881,3.1685426912215,298.087328865796));
#3175=CARTESIAN_POINT('Ctrl Pts',(0.538742812073637,3.17784345797606,298.090678454025));
#3176=CARTESIAN_POINT('Ctrl Pts',(0.424724139071017,3.19524737004199,298.098042776611));
#3177=CARTESIAN_POINT('Ctrl Pts',(0.362901179433595,3.20285783442598,298.102070491835));
#3178=CARTESIAN_POINT('Ctrl Pts',(0.169073936717036,3.22103436448897,298.114801315828));
#3179=CARTESIAN_POINT('Ctrl Pts',(0.0366216376400551,3.22526003050917,298.123655730661));
#3180=CARTESIAN_POINT('Ctrl Pts',(-0.284359912647403,3.21572371645284,298.145280995186));
#3181=CARTESIAN_POINT('Ctrl Pts',(-0.4721687516899,3.1935568241037,298.158085124294));
#3182=CARTESIAN_POINT('Ctrl Pts',(-0.69295846235032,3.14758283540607,298.172672001631));
#3183=CARTESIAN_POINT('Ctrl Pts',(-0.728821117846843,3.13947275392857,298.175025421685));
#3184=CARTESIAN_POINT('Ctrl Pts',(-0.785484913247391,3.12563528227853,298.178710394452));
#3185=CARTESIAN_POINT('Ctrl Pts',(-0.806379864384549,3.1203099272178,298.180061946459));
#3186=CARTESIAN_POINT('Ctrl Pts',(-0.847686556701125,3.10933971580286,298.182717178185));
#3187=CARTESIAN_POINT('Ctrl Pts',(-0.868099084774921,3.10370262601329,298.184021132953));
#3188=CARTESIAN_POINT('Ctrl Pts',(-0.922053377912032,3.08822875217649,298.187449562523));
#3189=CARTESIAN_POINT('Ctrl Pts',(-0.955494211869299,3.07804650530772,298.189555776803));
#3190=CARTESIAN_POINT('Ctrl Pts',(-1.14270937817302,3.01769689838389,298.20127542487));
#3191=CARTESIAN_POINT('Ctrl Pts',(-1.29271726027755,2.95654738589552,298.210398728571));
#3192=CARTESIAN_POINT('Ctrl Pts',(-1.63260663900358,2.78715428852557,298.231733711671));
#3193=CARTESIAN_POINT('Ctrl Pts',(-1.81731648951552,2.67039040889286,298.243891905099));
#3194=CARTESIAN_POINT('Ctrl Pts',(-2.03352108400273,2.50082714888708,298.260059563738));
#3195=CARTESIAN_POINT('Ctrl Pts',(-2.07728277742612,2.46459735513104,298.263441222975));
#3196=CARTESIAN_POINT('Ctrl Pts',(-2.14789787377132,2.40291868700456,298.269097808159));
#3197=CARTESIAN_POINT('Ctrl Pts',(-2.1753121492951,2.37812959574368,298.271346184632));
#3198=CARTESIAN_POINT('Ctrl Pts',(-2.22885849330394,2.32801017324282,298.275847074358));
#3199=CARTESIAN_POINT('Ctrl Pts',(-2.2549998534883,2.30269777472373,298.278098656237));
#3200=CARTESIAN_POINT('Ctrl Pts',(-2.31861487115342,2.2389777842165,298.283717402327));
#3201=CARTESIAN_POINT('Ctrl Pts',(-2.35556742763593,2.20006772484594,298.287106007648));
#3202=CARTESIAN_POINT('Ctrl Pts',(-2.52214717193582,2.01565412337334,298.302983058208));
#3203=CARTESIAN_POINT('Ctrl Pts',(-2.63936266769136,1.85952485963476,298.315949635673));
#3204=CARTESIAN_POINT('Ctrl Pts',(-2.84065140844619,1.53369778463225,298.341751046986));
#3205=CARTESIAN_POINT('Ctrl Pts',(-2.92534777304943,1.36523943220443,298.354519439996));
#3206=CARTESIAN_POINT('Ctrl Pts',(-3.00846715461208,1.15611405673199,298.369077942086));
#3207=CARTESIAN_POINT('Ctrl Pts',(-3.02148498959266,1.12165192923532,298.371436309191));
#3208=CARTESIAN_POINT('Ctrl Pts',(-3.04117983742346,1.06668054304194,298.375125835033));
#3209=CARTESIAN_POINT('Ctrl Pts',(-3.04824643673452,1.04631539520742,298.376477149375));
#3210=CARTESIAN_POINT('Ctrl Pts',(-3.06183137034291,1.00585897168002,298.379128831305));
#3211=CARTESIAN_POINT('Ctrl Pts',(-3.06835753176477,0.985771633100665,298.380429523657));
#3212=CARTESIAN_POINT('Ctrl Pts',(-3.08509886150542,0.932464666899898,298.38384281159));
#3213=CARTESIAN_POINT('Ctrl Pts',(-3.0949752756659,0.899140478698359,298.385937383));
#3214=CARTESIAN_POINT('Ctrl Pts',(-3.116048569681,0.823570460619718,298.390612683482));
#3215=CARTESIAN_POINT('Ctrl Pts',(-3.12692924982858,0.781243106843752,298.393179369342));
#3216=CARTESIAN_POINT('Ctrl Pts',(-3.16036602137312,0.63925240449213,298.401655807293));
#3217=CARTESIAN_POINT('Ctrl Pts',(-3.17904434828389,0.538735869891413,298.407439656722));
#3218=CARTESIAN_POINT('Ctrl Pts',(-3.22541621195218,0.200307297151154,298.426660769588));
#3219=CARTESIAN_POINT('Ctrl Pts',(-3.23138419072083,-0.0397437242021221,
298.439944322083));
#3220=CARTESIAN_POINT('Ctrl Pts',(-3.20602491621992,-0.332378027677306,
298.457263953187));
#3221=CARTESIAN_POINT('Ctrl Pts',(-3.19996455386814,-0.386390046878018,
298.460504720139));
#3222=CARTESIAN_POINT('Ctrl Pts',(-3.18805517551508,-0.472758488642186,
298.465770884098));
#3223=CARTESIAN_POINT('Ctrl Pts',(-3.18307151732941,-0.505224688292369,
298.467769591033));
#3224=CARTESIAN_POINT('Ctrl Pts',(-3.17156988229157,-0.573206376989585,
298.471997781393));
#3225=CARTESIAN_POINT('Ctrl Pts',(-3.16494954199224,-0.608699680032584,
298.474230177923));
#3226=CARTESIAN_POINT('Ctrl Pts',(-3.14730928595423,-0.69518557451247,298.479733833854));
#3227=CARTESIAN_POINT('Ctrl Pts',(-3.13564511615684,-0.746034807224774,
298.483024652436));
#3228=CARTESIAN_POINT('Ctrl Pts',(-3.10770952174123,-0.855548413743614,
298.490235642101));
#3229=CARTESIAN_POINT('Ctrl Pts',(-3.09099979309789,-0.914079377243734,
298.494167863774));
#3230=CARTESIAN_POINT('Ctrl Pts',(-3.03438304962176,-1.09303544343262,298.506429810837));
#3231=CARTESIAN_POINT('Ctrl Pts',(-2.98901868785504,-1.21159799003507,298.514898806429));
#3232=CARTESIAN_POINT('Ctrl Pts',(-2.85413239354378,-1.51007713582641,298.536946003867));
#3233=CARTESIAN_POINT('Ctrl Pts',(-2.75456388262891,-1.68487149835763,298.550597419637));
#3234=CARTESIAN_POINT('Ctrl Pts',(-2.61893242225138,-1.87845142726865,298.565869911451));
#3235=CARTESIAN_POINT('Ctrl Pts',(-2.59800598775317,-1.90728915540127,298.568148494384));
#3236=CARTESIAN_POINT('Ctrl Pts',(-2.56381318681165,-1.95280132526904,298.571742652846));
#3237=CARTESIAN_POINT('Ctrl Pts',(-2.55085278833936,-1.96970078607938,298.573076783023));
#3238=CARTESIAN_POINT('Ctrl Pts',(-2.52456211832076,-2.00328723034336,298.575725304862));
#3239=CARTESIAN_POINT('Ctrl Pts',(-2.51123160167491,-2.01997265281993,298.577039578494));
#3240=CARTESIAN_POINT('Ctrl Pts',(-2.47506274321663,-2.06433265720713,298.580533424514));
#3241=CARTESIAN_POINT('Ctrl Pts',(-2.45192585144059,-2.09176116182084,298.582693419418));
#3242=CARTESIAN_POINT('Ctrl Pts',(-2.32434259954537,-2.23798308577702,298.594242181843));
#3243=CARTESIAN_POINT('Ctrl Pts',(-2.21170583475831,-2.34936255906779,298.603168933322));
#3244=CARTESIAN_POINT('Ctrl Pts',(-1.92370770487942,-2.59499608423301,298.624435806898));
#3245=CARTESIAN_POINT('Ctrl Pts',(-1.74187899374605,-2.72038677972278,298.636716250659));
#3246=CARTESIAN_POINT('Ctrl Pts',(-1.5244468743339,-2.83953225480568,298.65130727442));
#3247=CARTESIAN_POINT('Ctrl Pts',(-1.50003654230719,-2.85250273788423,298.65294329802));
#3248=CARTESIAN_POINT('Ctrl Pts',(-1.47546399981363,-2.86515681032539,298.654589343883));
#3249=CARTESIAN_POINT('Origin',(0.,0.,294.689226550727));
#3250=CARTESIAN_POINT('',(-1.47546414420613,-2.86515673596787,300.152134095017));
#3251=CARTESIAN_POINT('',(-1.47546400147781,-2.86515680946839,299.907672586636));
#3252=CARTESIAN_POINT('',(-1.47546400239267,-2.86515680899727,294.689226550727));
#3253=CARTESIAN_POINT('Ctrl Pts',(-1.47546414420613,-2.86515673596787,300.152134095017));
#3254=CARTESIAN_POINT('Ctrl Pts',(-1.563549486761,-2.81979559989518,300.145496287807));
#3255=CARTESIAN_POINT('Ctrl Pts',(-1.64953114565584,-2.77037847724467,300.138924810279));
#3256=CARTESIAN_POINT('Ctrl Pts',(-1.76162338783503,-2.69887806569273,300.130351539397));
#3257=CARTESIAN_POINT('Ctrl Pts',(-1.78983046673973,-2.68025500284619,300.128193764278));
#3258=CARTESIAN_POINT('Ctrl Pts',(-1.83501423321666,-2.64939199023005,300.12474317954));
#3259=CARTESIAN_POINT('Ctrl Pts',(-1.85217332908825,-2.6374247270353,300.123434192876));
#3260=CARTESIAN_POINT('Ctrl Pts',(-1.88693843929308,-2.61267185608773,300.120786978898));
#3261=CARTESIAN_POINT('Ctrl Pts',(-1.90453376442025,-2.59987347830767,300.119449622142));
#3262=CARTESIAN_POINT('Ctrl Pts',(-1.95241894567294,-2.56429601269393,300.115812788393));
#3263=CARTESIAN_POINT('Ctrl Pts',(-1.98243962186252,-2.54115863340587,300.113535800539));
#3264=CARTESIAN_POINT('Ctrl Pts',(-2.14951247820355,-2.40762977437996,300.100837667517));
#3265=CARTESIAN_POINT('Ctrl Pts',(-2.27776360346689,-2.28667682631798,300.090977860896));
#3266=CARTESIAN_POINT('Ctrl Pts',(-2.53433845332124,-2.00157899001737,300.069450944227));
#3267=CARTESIAN_POINT('Ctrl Pts',(-2.65793109500705,-1.83427957220254,300.057806916586));
#3268=CARTESIAN_POINT('Ctrl Pts',(-2.79154219304184,-1.61126113042641,300.042450629321));
#3269=CARTESIAN_POINT('Ctrl Pts',(-2.81740177257449,-1.56560436968607,300.039317341756));
#3270=CARTESIAN_POINT('Ctrl Pts',(-2.85917251929353,-1.48746636985305,300.033960187568));
#3271=CARTESIAN_POINT('Ctrl Pts',(-2.87567275551391,-1.45531087345991,300.03175709769));
#3272=CARTESIAN_POINT('Ctrl Pts',(-2.90609608074538,-1.39348373611918,300.027520647675));
#3273=CARTESIAN_POINT('Ctrl Pts',(-2.92011419249179,-1.36386375146938,300.025490874761));
#3274=CARTESIAN_POINT('Ctrl Pts',(-2.95601117012331,-1.2849227275657,300.020078405565));
#3275=CARTESIAN_POINT('Ctrl Pts',(-2.9771065537306,-1.23525886905161,300.01667022153));
#3276=CARTESIAN_POINT('Ctrl Pts',(-3.0860306350114,-0.959803749766988,299.997740352056));
#3277=CARTESIAN_POINT('Ctrl Pts',(-3.14941701326185,-0.725220753789514,
299.981438264264));
#3278=CARTESIAN_POINT('Ctrl Pts',(-3.20112953441015,-0.386084907233361,
299.958316330828));
#3279=CARTESIAN_POINT('Ctrl Pts',(-3.21164531612068,-0.285706254992559,
299.951538956968));
#3280=CARTESIAN_POINT('Ctrl Pts',(-3.21992549833164,-0.141697775911958,
299.942031008696));
#3281=CARTESIAN_POINT('Ctrl Pts',(-3.22154088859554,-0.0983519814407669,
299.939197208208));
#3282=CARTESIAN_POINT('Ctrl Pts',(-3.22287046550643,-0.0204348434260564,
299.934167902587));
#3283=CARTESIAN_POINT('Ctrl Pts',(-3.22290433428755,0.0141241285302486,
299.931960074034));
#3284=CARTESIAN_POINT('Ctrl Pts',(-3.2220640859195,0.069746261029314,299.928450272112));
#3285=CARTESIAN_POINT('Ctrl Pts',(-3.22153921348952,0.090811243855519,299.927131146703));
#3286=CARTESIAN_POINT('Ctrl Pts',(-3.22005911864908,0.133423949830002,299.92448510169));
#3287=CARTESIAN_POINT('Ctrl Pts',(-3.21909412676297,0.154970130628407,299.923158720442));
#3288=CARTESIAN_POINT('Ctrl Pts',(-3.21588799795303,0.213421747348317,299.919587880599));
#3289=CARTESIAN_POINT('Ctrl Pts',(-3.21322791576597,0.250301968630703,299.917364562014));
#3290=CARTESIAN_POINT('Ctrl Pts',(-3.19352090477777,0.470614060514461,299.904218151561));
#3291=CARTESIAN_POINT('Ctrl Pts',(-3.1614042244661,0.652373624564809,299.893919936405));
#3292=CARTESIAN_POINT('Ctrl Pts',(-3.06192985806229,1.02538999835319,299.872253119217));
#3293=CARTESIAN_POINT('Ctrl Pts',(-2.99174081178703,1.21503727103232,299.860908909247));
#3294=CARTESIAN_POINT('Ctrl Pts',(-2.88170607968123,1.44381488041093,299.845908540881));
#3295=CARTESIAN_POINT('Ctrl Pts',(-2.85799253603054,1.49020453495757,299.842796556796));
#3296=CARTESIAN_POINT('Ctrl Pts',(-2.81597149556612,1.56771286593709,299.837464637358));
#3297=CARTESIAN_POINT('Ctrl Pts',(-2.79824614955375,1.59913646066605,299.835264998874));
#3298=CARTESIAN_POINT('Ctrl Pts',(-2.76338845158233,1.65857766393129,299.831027717092));
#3299=CARTESIAN_POINT('Ctrl Pts',(-2.74634799214967,1.68664405945773,299.828993535283));
#3300=CARTESIAN_POINT('Ctrl Pts',(-2.69996709038672,1.76046856764238,299.823550877854));
#3301=CARTESIAN_POINT('Ctrl Pts',(-2.66989378311293,1.80575150388964,299.820116373342));
#3302=CARTESIAN_POINT('Ctrl Pts',(-2.50131178302599,2.04617078075428,299.801344330845));
#3303=CARTESIAN_POINT('Ctrl Pts',(-2.34255822436219,2.22615411049026,299.785249657016));
#3304=CARTESIAN_POINT('Ctrl Pts',(-2.08965513658444,2.4555884531845,299.762232128189));
#3305=CARTESIAN_POINT('Ctrl Pts',(-2.010692449144,2.52065289047428,299.755358988234));
#3306=CARTESIAN_POINT('Ctrl Pts',(-1.89374977880329,2.60801453812505,299.745734560329));
#3307=CARTESIAN_POINT('Ctrl Pts',(-1.85820267959273,2.63345992915296,299.742877762231));
#3308=CARTESIAN_POINT('Ctrl Pts',(-1.79348007142165,2.67782650298746,299.737812441977));
#3309=CARTESIAN_POINT('Ctrl Pts',(-1.76449535217294,2.69701351888333,299.735591350453));
#3310=CARTESIAN_POINT('Ctrl Pts',(-1.71741506140514,2.72709529286136,299.732065831359));
#3311=CARTESIAN_POINT('Ctrl Pts',(-1.69951356148575,2.73828722986786,299.730743991563));
#3312=CARTESIAN_POINT('Ctrl Pts',(-1.66314479238028,2.76053075317411,299.728098049811));
#3313=CARTESIAN_POINT('Ctrl Pts',(-1.64467431508814,2.77157484058304,299.726774401516));
#3314=CARTESIAN_POINT('Ctrl Pts',(-1.59437233794269,2.80097203737478,299.723219960756));
#3315=CARTESIAN_POINT('Ctrl Pts',(-1.5623344686675,2.81896767743382,299.721009978234));
#3316=CARTESIAN_POINT('Ctrl Pts',(-1.3634378249976,2.92625488243654,299.707574915214));
#3317=CARTESIAN_POINT('Ctrl Pts',(-1.18927260801748,3.00126251697006,299.697012333321));
#3318=CARTESIAN_POINT('Ctrl Pts',(-0.823891189572074,3.1217824710916,299.675417485551));
#3319=CARTESIAN_POINT('Ctrl Pts',(-0.633101254567623,3.16599042953249,299.664415182304));
#3320=CARTESIAN_POINT('Ctrl Pts',(-0.387113354978648,3.1998525398595,299.649753894847));
#3321=CARTESIAN_POINT('Ctrl Pts',(-0.334568009085671,3.2057724199353,299.646597359688));
#3322=CARTESIAN_POINT('Ctrl Pts',(-0.245830945727075,3.21356436499495,299.641212613135));
#3323=CARTESIAN_POINT('Ctrl Pts',(-0.209709336233353,3.21612353835702,299.639005705586));
#3324=CARTESIAN_POINT('Ctrl Pts',(-0.1365482459055,3.22006917627843,299.634502048397));
#3325=CARTESIAN_POINT('Ctrl Pts',(-0.099512736678044,3.22142638592084,299.632204748356));
#3326=CARTESIAN_POINT('Ctrl Pts',(-0.00492897176134279,3.22325994949287,
299.62628996061));
#3327=CARTESIAN_POINT('Ctrl Pts',(0.0526217259274038,3.22283404611002,299.622645736504));
#3328=CARTESIAN_POINT('Ctrl Pts',(0.268206813217654,3.21546279294993,299.608817630297));
#3329=CARTESIAN_POINT('Ctrl Pts',(0.425654946869618,3.19842818758335,299.598347706023));
#3330=CARTESIAN_POINT('Ctrl Pts',(0.733662774720013,3.14195527748034,299.577317690514));
#3331=CARTESIAN_POINT('Ctrl Pts',(0.883910983267427,3.1030382457499,299.566792395836));
#3332=CARTESIAN_POINT('Ctrl Pts',(1.08234425028818,3.03605184173366,299.552876924668));
#3333=CARTESIAN_POINT('Ctrl Pts',(1.13346555452356,3.01733927063249,299.54929196399));
#3334=CARTESIAN_POINT('Ctrl Pts',(1.22205946120328,2.98234049843804,299.543105859657));
#3335=CARTESIAN_POINT('Ctrl Pts',(1.25974181782351,2.96662014274287,299.540483377253));
#3336=CARTESIAN_POINT('Ctrl Pts',(1.3175742873062,2.94119277749597,299.536482933941));
#3337=CARTESIAN_POINT('Ctrl Pts',(1.33793800893872,2.93198548907836,299.535079080511));
#3338=CARTESIAN_POINT('Ctrl Pts',(1.37661715070186,2.91401012489106,299.532423990696));
#3339=CARTESIAN_POINT('Ctrl Pts',(1.39494812330703,2.90527959748838,299.531170861429));
#3340=CARTESIAN_POINT('Ctrl Pts',(1.44159602572989,2.88251922051468,299.527992508266));
#3341=CARTESIAN_POINT('Ctrl Pts',(1.46979219288063,2.86824462617599,299.526081320729));
#3342=CARTESIAN_POINT('Ctrl Pts',(1.59676684173781,2.80159817281276,299.517499904559));
#3343=CARTESIAN_POINT('Ctrl Pts',(1.69299742679754,2.74451835174352,299.511064880895));
#3344=CARTESIAN_POINT('Ctrl Pts',(1.94642259942879,2.57578463469648,299.493791646811));
#3345=CARTESIAN_POINT('Ctrl Pts',(2.09687462939088,2.45486161550592,299.483148183455));
#3346=CARTESIAN_POINT('Ctrl Pts',(2.28932495904262,2.26950805608279,299.46788553351));
#3347=CARTESIAN_POINT('Ctrl Pts',(2.34120869852717,2.21594594865832,299.4635812));
#3348=CARTESIAN_POINT('Ctrl Pts',(2.43172984129206,2.1157657190864,299.455660706836));
#3349=CARTESIAN_POINT('Ctrl Pts',(2.47100016999023,2.06976619079909,299.452069816462));
#3350=CARTESIAN_POINT('Ctrl Pts',(2.53255683337475,1.99341114157365,299.446162602071));
#3351=CARTESIAN_POINT('Ctrl Pts',(2.55564695804178,1.96372109514022,299.443878140299));
#3352=CARTESIAN_POINT('Ctrl Pts',(2.59948181126903,1.9052739002946,299.439400951123));
#3353=CARTESIAN_POINT('Ctrl Pts',(2.62028202517081,1.87656502013045,299.437210796515));
#3354=CARTESIAN_POINT('Ctrl Pts',(2.66952716259211,1.80618044168319,299.431859886711));
#3355=CARTESIAN_POINT('Ctrl Pts',(2.69747440717476,1.76416961563188,299.428681354976));
#3356=CARTESIAN_POINT('Ctrl Pts',(2.81349638678403,1.5805571182932,299.414846469962));
#3357=CARTESIAN_POINT('Ctrl Pts',(2.89148340255457,1.43291071217499,299.403846177885));
#3358=CARTESIAN_POINT('Ctrl Pts',(3.02127957829406,1.13297075735029,299.381919913077));
#3359=CARTESIAN_POINT('Ctrl Pts',(3.07382850959044,0.981494700323993,299.371041239186));
#3360=CARTESIAN_POINT('Ctrl Pts',(3.12907985012651,0.773324692873389,299.356723720829));
#3361=CARTESIAN_POINT('Ctrl Pts',(3.14188151554877,0.719550503793197,299.353081631265));
#3362=CARTESIAN_POINT('Ctrl Pts',(3.16181781622192,0.625083570764121,299.346809126808));
#3363=CARTESIAN_POINT('Ctrl Pts',(3.16956495888623,0.584533744754777,299.344156608327));
#3364=CARTESIAN_POINT('Ctrl Pts',(3.18031758487748,0.52172890128881,299.340120865111));
#3365=CARTESIAN_POINT('Ctrl Pts',(3.18387295720959,0.499573865566821,299.338711063671));
#3366=CARTESIAN_POINT('Ctrl Pts',(3.19019780197776,0.457346692858114,299.336052601732));
#3367=CARTESIAN_POINT('Ctrl Pts',(3.19300984291246,0.437282716274429,299.334801915709));
#3368=CARTESIAN_POINT('Ctrl Pts',(3.19969069695675,0.386108449562979,299.331641011643));
#3369=CARTESIAN_POINT('Ctrl Pts',(3.20329524089861,0.354964864261157,299.32974450534));
#3370=CARTESIAN_POINT('Ctrl Pts',(3.21722622669429,0.217000837729855,299.321443630263));
#3371=CARTESIAN_POINT('Ctrl Pts',(3.22266871063748,0.109747374945496,299.31525530431));
#3372=CARTESIAN_POINT('Ctrl Pts',(3.22288674166129,-0.181375703593998,299.298715214201));
#3373=CARTESIAN_POINT('Ctrl Pts',(3.20730257840436,-0.364840062766869,299.288552665414));
#3374=CARTESIAN_POINT('Ctrl Pts',(3.15638739802366,-0.66103328564887,299.271451557693));
#3375=CARTESIAN_POINT('Ctrl Pts',(3.13037423414779,-0.774919255549078,299.264707235851));
#3376=CARTESIAN_POINT('Ctrl Pts',(3.08647928354816,-0.928218343966984,299.255240031375));
#3377=CARTESIAN_POINT('Ctrl Pts',(3.07390056120917,-0.969060757186082,299.252679554835));
#3378=CARTESIAN_POINT('Ctrl Pts',(3.04939183864144,-1.04335388392142,299.247944822355));
#3379=CARTESIAN_POINT('Ctrl Pts',(3.03771380356277,-1.0768809623489,299.245778857995));
#3380=CARTESIAN_POINT('Ctrl Pts',(3.01256079215715,-1.14542676452772,299.241286740243));
#3381=CARTESIAN_POINT('Ctrl Pts',(2.99902339712373,-1.18041665407409,299.238958823198));
#3382=CARTESIAN_POINT('Ctrl Pts',(2.96226460620396,-1.27070964415948,299.232856992934));
#3383=CARTESIAN_POINT('Ctrl Pts',(2.93810554754108,-1.32561293042703,299.229052883889));
#3384=CARTESIAN_POINT('Ctrl Pts',(2.88087507068635,-1.44641221240006,299.22046718668));
#3385=CARTESIAN_POINT('Ctrl Pts',(2.84704655955309,-1.51191075251473,299.215663519429));
#3386=CARTESIAN_POINT('Ctrl Pts',(2.71932021150384,-1.73970033067975,299.198440382127));
#3387=CARTESIAN_POINT('Ctrl Pts',(2.61354781484821,-1.89489278614232,299.185718988243));
#3388=CARTESIAN_POINT('Ctrl Pts',(2.42001534349954,-2.13158114860275,299.165179933183));
#3389=CARTESIAN_POINT('Ctrl Pts',(2.34013868835361,-2.21897910523336,299.157306944371));
#3390=CARTESIAN_POINT('Ctrl Pts',(2.23288762038897,-2.32407924762077,299.147646430006));
#3391=CARTESIAN_POINT('Ctrl Pts',(2.2098149912666,-2.34602842138877,299.145617527318));
#3392=CARTESIAN_POINT('Ctrl Pts',(2.17147316854219,-2.38143565090629,299.142331161196));
#3393=CARTESIAN_POINT('Ctrl Pts',(2.15639543694034,-2.39509713471953,299.141059786481));
#3394=CARTESIAN_POINT('Ctrl Pts',(2.12454903300024,-2.42340765088651,299.138419682113));
#3395=CARTESIAN_POINT('Ctrl Pts',(2.10775620636334,-2.43802729191267,299.137052921841));
#3396=CARTESIAN_POINT('Ctrl Pts',(2.06006401347751,-2.47868644423725,299.133237660296));
#3397=CARTESIAN_POINT('Ctrl Pts',(2.02882352182033,-2.50432139946177,299.130815467557));
#3398=CARTESIAN_POINT('Ctrl Pts',(1.95499372939945,-2.56261513874834,299.125245815627));
#3399=CARTESIAN_POINT('Ctrl Pts',(1.91205384335592,-2.59481164683851,299.122121803894));
#3400=CARTESIAN_POINT('Ctrl Pts',(1.74571765018845,-2.71315885429767,299.110369589579));
#3401=CARTESIAN_POINT('Ctrl Pts',(1.61714226009152,-2.791704911298,299.101986996676));
#3402=CARTESIAN_POINT('Ctrl Pts',(1.33778419675828,-2.93656424592635,299.084304194234));
#3403=CARTESIAN_POINT('Ctrl Pts',(1.18647494667525,-3.00089094599694,299.075010857996));
#3404=CARTESIAN_POINT('Ctrl Pts',(0.976417839463468,-3.07181319257301,299.061974038049));
#3405=CARTESIAN_POINT('Ctrl Pts',(0.9214235382365,-3.08875479156811,299.05855074832));
#3406=CARTESIAN_POINT('Ctrl Pts',(0.830313110490968,-3.11417259575874,299.052846266156));
#3407=CARTESIAN_POINT('Ctrl Pts',(0.794450742439805,-3.12351383264113,299.050592694904));
#3408=CARTESIAN_POINT('Ctrl Pts',(0.723241526182453,-3.14075636737339,299.046097978202));
#3409=CARTESIAN_POINT('Ctrl Pts',(0.687906730818511,-3.14868433279057,299.043858047684));
#3410=CARTESIAN_POINT('Ctrl Pts',(0.600663306123015,-3.16672027545137,299.038300921395));
#3411=CARTESIAN_POINT('Ctrl Pts',(0.548626613046161,-3.17614893122665,299.034963245026));
#3412=CARTESIAN_POINT('Ctrl Pts',(0.303097695713372,-3.21442323295909,299.019098206603));
#3413=CARTESIAN_POINT('Ctrl Pts',(0.107496798203785,-3.22688845579623,299.006085787622));
#3414=CARTESIAN_POINT('Ctrl Pts',(-0.276994704810866,-3.21638578880807,
298.980175479974));
#3415=CARTESIAN_POINT('Ctrl Pts',(-0.465180787409814,-3.19460161136501,
298.967344848395));
#3416=CARTESIAN_POINT('Ctrl Pts',(-0.686377900808624,-3.14902425866946,
298.952735368959));
#3417=CARTESIAN_POINT('Ctrl Pts',(-0.722247728320832,-3.14099138520554,
298.950382314337));
#3418=CARTESIAN_POINT('Ctrl Pts',(-0.778892041586941,-3.12728443526204,
298.946700139958));
#3419=CARTESIAN_POINT('Ctrl Pts',(-0.799759603834225,-3.12201303458973,
298.945350957575));
#3420=CARTESIAN_POINT('Ctrl Pts',(-0.840987293683504,-3.11115791119713,
298.94270204384));
#3421=CARTESIAN_POINT('Ctrl Pts',(-0.861348332266915,-3.10558243687959,
298.941402004251));
#3422=CARTESIAN_POINT('Ctrl Pts',(-0.915074949881425,-3.09030139989273,
298.937989748997));
#3423=CARTESIAN_POINT('Ctrl Pts',(-0.948341854935828,-3.08025532207555,
298.93589555004));
#3424=CARTESIAN_POINT('Ctrl Pts',(-1.02305920641151,-3.05636655722115,298.931220797139));
#3425=CARTESIAN_POINT('Ctrl Pts',(-1.06440411298453,-3.0422147999709,298.928654282202));
#3426=CARTESIAN_POINT('Ctrl Pts',(-1.20143690815107,-2.99217462264578,298.920177123254));
#3427=CARTESIAN_POINT('Ctrl Pts',(-1.29570768167465,-2.95257573994885,298.914392369835));
#3428=CARTESIAN_POINT('Ctrl Pts',(-1.4173446430655,-2.8945315868833,298.90680829297));
#3429=CARTESIAN_POINT('Ctrl Pts',(-1.44652186378979,-2.88006108465439,298.904979765819));
#3430=CARTESIAN_POINT('Ctrl Pts',(-1.47546409036594,-2.86515676369385,298.903152516993));
#3431=CARTESIAN_POINT('',(3.22274998327137,0.000328366225831933,299.061455114234));
#3432=CARTESIAN_POINT('Ctrl Pts',(-1.47546399981363,-2.86515681032539,298.654589343883));
#3433=CARTESIAN_POINT('Ctrl Pts',(-1.44972727176912,-2.8784104010419,298.656313375279));
#3434=CARTESIAN_POINT('Ctrl Pts',(-1.42381259905786,-2.89131688948619,298.6580484028));
#3435=CARTESIAN_POINT('Ctrl Pts',(-1.36446682477198,-2.91988191139373,298.662022252458));
#3436=CARTESIAN_POINT('Ctrl Pts',(-1.33093520187307,-2.93531794016742,298.66426797716));
#3437=CARTESIAN_POINT('Ctrl Pts',(-1.26382007437086,-2.96482744453382,298.668767485804));
#3438=CARTESIAN_POINT('Ctrl Pts',(-1.23024850074144,-2.97891446896464,298.671020406907));
#3439=CARTESIAN_POINT('Ctrl Pts',(-1.14648503000512,-3.01240515599955,298.676650214486));
#3440=CARTESIAN_POINT('Ctrl Pts',(-1.09603361673257,-3.03112561855672,298.68004875204));
#3441=CARTESIAN_POINT('Ctrl Pts',(-0.868060424748604,-3.1092814454528,298.695447848269));
#3442=CARTESIAN_POINT('Ctrl Pts',(-0.686052861443158,-3.15443713918839,
298.707884473109));
#3443=CARTESIAN_POINT('Ctrl Pts',(-0.306875813562086,-3.21413052489826,
298.733726884096));
#3444=CARTESIAN_POINT('Ctrl Pts',(-0.110167435728297,-3.22686848774799,
298.747094095232));
#3445=CARTESIAN_POINT('Ctrl Pts',(0.122538922243097,-3.22062147587102,298.762141870928));
#3446=CARTESIAN_POINT('Ctrl Pts',(0.158577091441751,-3.21904831123245,298.764449564213));
#3447=CARTESIAN_POINT('Ctrl Pts',(0.215940807579819,-3.21557847975082,298.768078926574));
#3448=CARTESIAN_POINT('Ctrl Pts',(0.237286024440114,-3.2140738625771,298.769419713178));
#3449=CARTESIAN_POINT('Ctrl Pts',(0.279820894036702,-3.21064953226938,298.772070045707));
#3450=CARTESIAN_POINT('Ctrl Pts',(0.301009642550687,-3.20873236670442,298.773379635183));
#3451=CARTESIAN_POINT('Ctrl Pts',(0.357483491662,-3.20305824830348,298.776845210373));
#3452=CARTESIAN_POINT('Ctrl Pts',(0.392729130563988,-3.19892804677135,298.778982175235));
#3453=CARTESIAN_POINT('Ctrl Pts',(0.472436474736355,-3.18825035829915,298.783770401538));
#3454=CARTESIAN_POINT('Ctrl Pts',(0.516844370135017,-3.18135330070173,298.786406583031));
#3455=CARTESIAN_POINT('Ctrl Pts',(0.666768876743215,-3.15484592176801,298.795242262176));
#3456=CARTESIAN_POINT('Ctrl Pts',(0.771449192611776,-3.13089478736509,298.801304465707));
#3457=CARTESIAN_POINT('Ctrl Pts',(1.09498089377746,-3.03965396986981,298.820202799356));
#3458=CARTESIAN_POINT('Ctrl Pts',(1.30795679462404,-2.95427131424047,298.832931691854));
#3459=CARTESIAN_POINT('Ctrl Pts',(1.5592801309835,-2.82096852048813,298.849686957103));
#3460=CARTESIAN_POINT('Ctrl Pts',(1.60778327113594,-2.79360883740029,298.85300422155));
#3461=CARTESIAN_POINT('Ctrl Pts',(1.68707394293094,-2.74613346000209,298.858582726813));
#3462=CARTESIAN_POINT('Ctrl Pts',(1.71827040180665,-2.72672223128069,298.860818947206));
#3463=CARTESIAN_POINT('Ctrl Pts',(1.77982571474049,-2.68694508810186,298.865318465518));
#3464=CARTESIAN_POINT('Ctrl Pts',(1.81018345625124,-2.66658755053654,298.867581230052));
#3465=CARTESIAN_POINT('Ctrl Pts',(1.88503625403199,-2.61452488125141,298.873273887736));
#3466=CARTESIAN_POINT('Ctrl Pts',(1.92908232715173,-2.58219728921272,298.876726523632));
#3467=CARTESIAN_POINT('Ctrl Pts',(2.11820279416264,-2.43585235974076,298.892017668719));
#3468=CARTESIAN_POINT('Ctrl Pts',(2.25413637994349,-2.31063021183482,298.904275603743));
#3469=CARTESIAN_POINT('Ctrl Pts',(2.5121798699909,-2.02836534794506,298.930021874429));
#3470=CARTESIAN_POINT('Ctrl Pts',(2.63202143352579,-1.87023694225259,298.943479788305));
#3471=CARTESIAN_POINT('Ctrl Pts',(2.75557590075299,-1.67158913535168,298.95859983779));
#3472=CARTESIAN_POINT('Ctrl Pts',(2.77404353435776,-1.64075942629812,298.960898667214));
#3473=CARTESIAN_POINT('Ctrl Pts',(2.80266401943303,-1.59111548070182,298.964517321434));
#3474=CARTESIAN_POINT('Ctrl Pts',(2.81315154979447,-1.57249880639375,298.96585609137));
#3475=CARTESIAN_POINT('Ctrl Pts',(2.83372093834934,-1.53512107991172,298.968505713402));
#3476=CARTESIAN_POINT('Ctrl Pts',(2.84380351986709,-1.51636165969508,298.969816562622));
#3477=CARTESIAN_POINT('Ctrl Pts',(2.87024022903925,-1.46598284603505,298.973290162266));
#3478=CARTESIAN_POINT('Ctrl Pts',(2.88625814159511,-1.43418926538341,298.975433728949));
#3479=CARTESIAN_POINT('Ctrl Pts',(2.96857206817698,-1.26383897929995,298.986696944379));
#3480=CARTESIAN_POINT('Ctrl Pts',(3.02543233258286,-1.12092726726277,298.995380459747));
#3481=CARTESIAN_POINT('Ctrl Pts',(3.13875471800757,-0.7637017781328,299.016446315585));
#3482=CARTESIAN_POINT('Ctrl Pts',(3.18374527431879,-0.546606845896657,299.028754599677));
#3483=CARTESIAN_POINT('Ctrl Pts',(3.21199439995888,-0.269310680461309,299.045128815724));
#3484=CARTESIAN_POINT('Ctrl Pts',(3.21629489894568,-0.211855621199054,299.048552849423));
#3485=CARTESIAN_POINT('Ctrl Pts',(3.22043839029637,-0.125423264005401,299.053766033411));
#3486=CARTESIAN_POINT('Ctrl Pts',(3.22143444773672,-0.0965113372770463,
299.05552024537));
#3487=CARTESIAN_POINT('Ctrl Pts',(3.22251600548125,-0.0449535281750034,
299.058668704482));
#3488=CARTESIAN_POINT('Ctrl Pts',(3.22275229016343,-0.0223126235551124,
299.060058250793));
#3489=CARTESIAN_POINT('Ctrl Pts',(3.22274998327137,0.000328366225831933,
299.061455114234));
#3490=CARTESIAN_POINT('Ctrl Pts',(3.2227499833101,0.000327985858891378,
299.061455090767));
#3491=CARTESIAN_POINT('Ctrl Pts',(3.22274652943001,0.0342654002378796,299.063548900761));
#3492=CARTESIAN_POINT('Ctrl Pts',(3.22220700613506,0.0681998290130912,299.065658974486));
#3493=CARTESIAN_POINT('Ctrl Pts',(3.21947014498759,0.154528700673276,299.071071128188));
#3494=CARTESIAN_POINT('Ctrl Pts',(3.2165298177619,0.206887808251486,299.074395187485));
#3495=CARTESIAN_POINT('Ctrl Pts',(3.19495845765172,0.474277662394748,299.09159017247));
#3496=CARTESIAN_POINT('Ctrl Pts',(3.15603891383566,0.687089508949695,299.10605626149));
#3497=CARTESIAN_POINT('Ctrl Pts',(3.05030848821211,1.05310533397084,299.131749186655));
#3498=CARTESIAN_POINT('Ctrl Pts',(2.99231729381699,1.2080806206243,299.142887430541));
#3499=CARTESIAN_POINT('Ctrl Pts',(2.90851574812353,1.3884472147167,299.155709639974));
#3500=CARTESIAN_POINT('Ctrl Pts',(2.89386167901502,1.41873687176191,299.157857365973));
#3501=CARTESIAN_POINT('Ctrl Pts',(2.86933862323411,1.46746391293589,299.161296922416));
#3502=CARTESIAN_POINT('Ctrl Pts',(2.85976010165921,1.48604398016733,299.162604724947));
#3503=CARTESIAN_POINT('Ctrl Pts',(2.83980893666348,1.52383706194522,299.165255281266));
#3504=CARTESIAN_POINT('Ctrl Pts',(2.82942059866414,1.54304028667318,299.16659707343));
#3505=CARTESIAN_POINT('Ctrl Pts',(2.80032139422189,1.59554907856148,299.170256305141));
#3506=CARTESIAN_POINT('Ctrl Pts',(2.78121172208303,1.62863083914335,299.172550820575));
#3507=CARTESIAN_POINT('Ctrl Pts',(2.69634853721565,1.76969011750964,299.182321221369));
#3508=CARTESIAN_POINT('Ctrl Pts',(2.62485627100743,1.87409545685446,299.189521128991));
#3509=CARTESIAN_POINT('Ctrl Pts',(2.44154800288276,2.11064665212321,299.206395487783));
#3510=CARTESIAN_POINT('Ctrl Pts',(2.32487318237436,2.23851501047242,299.215991761999));
#3511=CARTESIAN_POINT('Ctrl Pts',(2.14650908015825,2.40492706762266,299.229957032947));
#3512=CARTESIAN_POINT('Ctrl Pts',(2.09291929588547,2.45170621938392,299.234072338396));
#3513=CARTESIAN_POINT('Ctrl Pts',(1.99253876365373,2.5336385803422,299.241685753729));
#3514=CARTESIAN_POINT('Ctrl Pts',(1.94625412153623,2.56936362946208,299.245161809221));
#3515=CARTESIAN_POINT('Ctrl Pts',(1.86892391032431,2.62576256718452,299.250931633346));
#3516=CARTESIAN_POINT('Ctrl Pts',(1.83844487782098,2.64719207796599,299.253196496412));
#3517=CARTESIAN_POINT('Ctrl Pts',(1.77803018218675,2.68812241572455,299.257671803833));
#3518=CARTESIAN_POINT('Ctrl Pts',(1.7481281789436,2.70766341351952,299.259880323221));
#3519=CARTESIAN_POINT('Ctrl Pts',(1.67396666145783,2.75438750086574,299.26534497329));
#3520=CARTESIAN_POINT('Ctrl Pts',(1.62936419624911,2.78100462330133,299.268620719597));
#3521=CARTESIAN_POINT('Ctrl Pts',(1.36070805727037,2.93264695287077,299.288299071401));
#3522=CARTESIAN_POINT('Ctrl Pts',(1.12304640696586,3.03161158339221,299.305600120804));
#3523=CARTESIAN_POINT('Ctrl Pts',(0.785279453879957,3.12704089828685,299.329239937053));
#3524=CARTESIAN_POINT('Ctrl Pts',(0.693244638444545,3.14872389556241,299.335577660602));
#3525=CARTESIAN_POINT('Ctrl Pts',(0.559341962365844,3.17411394233356,299.344548507362));
#3526=CARTESIAN_POINT('Ctrl Pts',(0.518148570284986,3.18109809877438,299.347274453156));
#3527=CARTESIAN_POINT('Ctrl Pts',(0.44358771873394,3.19225268942585,299.352134743905));
#3528=CARTESIAN_POINT('Ctrl Pts',(0.410268840565864,3.19670564467387,299.354280277517));
#3529=CARTESIAN_POINT('Ctrl Pts',(0.35613154876545,3.20308047946914,299.357717304906));
#3530=CARTESIAN_POINT('Ctrl Pts',(0.335353965326037,3.20532245422802,299.359024726494));
#3531=CARTESIAN_POINT('Ctrl Pts',(0.292817714721626,3.20949410429793,299.361675489255));
#3532=CARTESIAN_POINT('Ctrl Pts',(0.271058544082364,3.21140498032574,299.363017853156));
#3533=CARTESIAN_POINT('Ctrl Pts',(0.21114739735927,3.2160530557697,299.366680538027));
#3534=CARTESIAN_POINT('Ctrl Pts',(0.172962378619341,3.21833260831637,299.368977862752));
#3535=CARTESIAN_POINT('Ctrl Pts',(-0.0367391129070247,3.22710795688053,
299.381434179051));
#3536=CARTESIAN_POINT('Ctrl Pts',(-0.208539857577076,3.22057428817795,299.3910627984));
#3537=CARTESIAN_POINT('Ctrl Pts',(-0.520108818447957,3.18367562584064,299.408673204732));
#3538=CARTESIAN_POINT('Ctrl Pts',(-0.659937138630424,3.15765484489247,299.416632983012));
#3539=CARTESIAN_POINT('Ctrl Pts',(-0.860212983691056,3.10649789293809,299.428522095241));
#3540=CARTESIAN_POINT('Ctrl Pts',(-0.922341162682467,3.08862131492622,299.432279418562));
#3541=CARTESIAN_POINT('Ctrl Pts',(-1.03581087776999,3.05224287121845,299.439304573561));
#3542=CARTESIAN_POINT('Ctrl Pts',(-1.08730109076792,3.03428188383167,299.442555827765));
#3543=CARTESIAN_POINT('Ctrl Pts',(-1.17248507537425,3.00212105285813,299.448055174808));
#3544=CARTESIAN_POINT('Ctrl Pts',(-1.20643833823916,2.98863822465511,299.450279805762));
#3545=CARTESIAN_POINT('Ctrl Pts',(-1.27408318216367,2.96043592938583,299.454781494208));
#3546=CARTESIAN_POINT('Ctrl Pts',(-1.30776664591104,2.94571130162186,299.457058456034));
#3547=CARTESIAN_POINT('Ctrl Pts',(-1.39191632125742,2.90719773986043,299.462839738995));
#3548=CARTESIAN_POINT('Ctrl Pts',(-1.44202878292749,2.8826692714849,299.46636835399));
#3549=CARTESIAN_POINT('Ctrl Pts',(-1.69354036726437,2.75136266606126,299.484529315101));
#3550=CARTESIAN_POINT('Ctrl Pts',(-1.88381382441009,2.62474594363358,299.499834162193));
#3551=CARTESIAN_POINT('Ctrl Pts',(-2.14202141941021,2.41028582596662,299.522467306961));
#3552=CARTESIAN_POINT('Ctrl Pts',(-2.22142777066103,2.33730489266956,299.529722523681));
#3553=CARTESIAN_POINT('Ctrl Pts',(-2.32862346381739,2.22837588240021,299.53981012481));
#3554=CARTESIAN_POINT('Ctrl Pts',(-2.35954122060311,2.19561196591743,299.542757171771));
#3555=CARTESIAN_POINT('Ctrl Pts',(-2.41361158563693,2.13585115751491,299.547963874209));
#3556=CARTESIAN_POINT('Ctrl Pts',(-2.43702329695914,2.10909903505091,299.550237075028));
#3557=CARTESIAN_POINT('Ctrl Pts',(-2.47373989080687,2.06571576246227,299.553825279728));
#3558=CARTESIAN_POINT('Ctrl Pts',(-2.48733028638676,2.04933129748226,299.555158715314));
#3559=CARTESIAN_POINT('Ctrl Pts',(-2.51424196133368,2.01622466805292,299.557807836605));
#3560=CARTESIAN_POINT('Ctrl Pts',(-2.52756117562432,1.99950221672883,299.559123370618));
#3561=CARTESIAN_POINT('Ctrl Pts',(-2.5628531317649,1.95427646307167,299.562624899302));
#3562=CARTESIAN_POINT('Ctrl Pts',(-2.58451708114854,1.92553482567744,299.564791164076));
#3563=CARTESIAN_POINT('Ctrl Pts',(-2.72188392441937,1.73679319741942,299.578681682843));
#3564=CARTESIAN_POINT('Ctrl Pts',(-2.82316845962759,1.56679295450636,299.589675973107));
#3565=CARTESIAN_POINT('Ctrl Pts',(-2.96356564030094,1.27274189386293,299.607969050815));
#3566=CARTESIAN_POINT('Ctrl Pts',(-3.01189893099362,1.15371381949891,299.615193673971));
#3567=CARTESIAN_POINT('Ctrl Pts',(-3.07262239223831,0.974095302863697,299.626128825142));
#3568=CARTESIAN_POINT('Ctrl Pts',(-3.09058142087567,0.915519471101641,299.629698847361));
#3569=CARTESIAN_POINT('Ctrl Pts',(-3.12079038022706,0.805935910786828,299.636413511808));
#3570=CARTESIAN_POINT('Ctrl Pts',(-3.13348544947862,0.755072031760421,299.639544146113));
#3571=CARTESIAN_POINT('Ctrl Pts',(-3.15283208023271,0.668636640488964,299.644899835209));
#3572=CARTESIAN_POINT('Ctrl Pts',(-3.16013549121602,0.633220813553157,299.64710420046));
#3573=CARTESIAN_POINT('Ctrl Pts',(-3.17292822332172,0.565439008533792,299.651345267361));
#3574=CARTESIAN_POINT('Ctrl Pts',(-3.17852198387097,0.533097229954114,299.653378409875));
#3575=CARTESIAN_POINT('Ctrl Pts',(-3.19202971807472,0.447206447929462,299.658805451542));
#3576=CARTESIAN_POINT('Ctrl Pts',(-3.19908993931695,0.39353568476881,299.662225051569));
#3577=CARTESIAN_POINT('Ctrl Pts',(-3.23021349317849,0.0999230793525244,
299.681096782862));
#3578=CARTESIAN_POINT('Ctrl Pts',(-3.22863505367647,-0.141930876552373,
299.697320409317));
#3579=CARTESIAN_POINT('Ctrl Pts',(-3.18812008460518,-0.481958291917196,
299.720401367959));
#3580=CARTESIAN_POINT('Ctrl Pts',(-3.17138333488818,-0.581999202259457,
299.72721350014));
#3581=CARTESIAN_POINT('Ctrl Pts',(-3.14076408719736,-0.723609758698783,
299.736764485859));
#3582=CARTESIAN_POINT('Ctrl Pts',(-3.13070964948847,-0.765942270748718,
299.739607364256));
#3583=CARTESIAN_POINT('Ctrl Pts',(-3.11111494654605,-0.841594533335596,
299.74465130694));
#3584=CARTESIAN_POINT('Ctrl Pts',(-3.10188863376593,-0.874988395979888,
299.746864783742));
#3585=CARTESIAN_POINT('Ctrl Pts',(-3.08617850944212,-0.928474576100684,
299.750382134578));
#3586=CARTESIAN_POINT('Ctrl Pts',(-3.08003282585468,-0.948662581466748,
299.751703260386));
#3587=CARTESIAN_POINT('Ctrl Pts',(-3.06720178168864,-0.989371772621045,
299.754352162033));
#3588=CARTESIAN_POINT('Ctrl Pts',(-3.06050773848367,-1.009888962818,299.755679415671));
#3589=CARTESIAN_POINT('Ctrl Pts',(-3.04178754238398,-1.06536991872102,299.759251187829));
#3590=CARTESIAN_POINT('Ctrl Pts',(-3.02936467036833,-1.10019746737571,299.761474577198));
#3591=CARTESIAN_POINT('Ctrl Pts',(-2.95130406516198,-1.30768480066771,299.774650452702));
#3592=CARTESIAN_POINT('Ctrl Pts',(-2.87151386680793,-1.47467219581102,299.784974557556));
#3593=CARTESIAN_POINT('Ctrl Pts',(-2.67594058513953,-1.80716927650832,299.806624503734));
#3594=CARTESIAN_POINT('Ctrl Pts',(-2.55806070616615,-1.97049076739934,299.817925501167));
#3595=CARTESIAN_POINT('Ctrl Pts',(-2.391343347136,-2.16109344518877,299.832886243998));
#3596=CARTESIAN_POINT('Ctrl Pts',(-2.35599196947165,-2.19957933981397,299.836007359242));
#3597=CARTESIAN_POINT('Ctrl Pts',(-2.29464016256247,-2.26319454798497,299.841351784131));
#3598=CARTESIAN_POINT('Ctrl Pts',(-2.26912351267697,-2.28877726322254,299.843554619228));
#3599=CARTESIAN_POINT('Ctrl Pts',(-2.21959650962692,-2.33679011411177,299.847796089334));
#3600=CARTESIAN_POINT('Ctrl Pts',(-2.19566259756052,-2.35929276184724,299.849831221558));
#3601=CARTESIAN_POINT('Ctrl Pts',(-2.13125957688887,-2.41801560520044,299.855271832299));
#3602=CARTESIAN_POINT('Ctrl Pts',(-2.09021316436199,-2.45358415793376,299.858703254716));
#3603=CARTESIAN_POINT('Ctrl Pts',(-1.87125441526666,-2.63383874863234,299.876833425788));
#3604=CARTESIAN_POINT('Ctrl Pts',(-1.67921620378575,-2.7602309503553,299.892218230902));
#3605=CARTESIAN_POINT('Ctrl Pts',(-1.47546400147781,-2.86515680946839,299.907672586636));
#3606=CARTESIAN_POINT('Origin',(0.,0.,294.689226550727));
#3607=CARTESIAN_POINT('',(-1.47546400249216,-2.86515680894603,301.40644069294));
#3608=CARTESIAN_POINT('',(-1.47546399521001,-2.86515681269611,301.158594111703));
#3609=CARTESIAN_POINT('',(-1.47546400239267,-2.86515680899727,294.689226550727));
#3610=CARTESIAN_POINT('',(3.22274884483193,-0.00272866899239652,300.5603484081));
#3611=CARTESIAN_POINT('Ctrl Pts',(-1.47546400249216,-2.86515680894603,301.40644069294));
#3612=CARTESIAN_POINT('Ctrl Pts',(-1.48048779144244,-2.86256971851904,301.406095014753));
#3613=CARTESIAN_POINT('Ctrl Pts',(-1.48550478569221,-2.85996941000239,301.405748883669));
#3614=CARTESIAN_POINT('Ctrl Pts',(-1.52255103390791,-2.84064455585854,301.403186139525));
#3615=CARTESIAN_POINT('Ctrl Pts',(-1.55430275391081,-2.82339616904349,301.400951628733));
#3616=CARTESIAN_POINT('Ctrl Pts',(-1.63139331994373,-2.77982399220617,301.395429324958));
#3617=CARTESIAN_POINT('Ctrl Pts',(-1.67639146020706,-2.75292149557001,301.39212163822));
#3618=CARTESIAN_POINT('Ctrl Pts',(-1.7725252509366,-2.69221599731516,301.384865802181));
#3619=CARTESIAN_POINT('Ctrl Pts',(-1.82339246276776,-2.65802782598722,301.380905315219));
#3620=CARTESIAN_POINT('Ctrl Pts',(-1.97781921567345,-2.54771709546525,301.368503391277));
#3621=CARTESIAN_POINT('Ctrl Pts',(-2.07781750929126,-2.46684027798489,301.359919053805));
#3622=CARTESIAN_POINT('Ctrl Pts',(-2.31836096538013,-2.24726693192574,301.337992074979));
#3623=CARTESIAN_POINT('Ctrl Pts',(-2.45150570599166,-2.1012223433221,301.324589002491));
#3624=CARTESIAN_POINT('Ctrl Pts',(-2.59218619337671,-1.91519830870355,301.309513481265));
#3625=CARTESIAN_POINT('Ctrl Pts',(-2.6134213391613,-1.88611849344987,301.307210001328));
#3626=CARTESIAN_POINT('Ctrl Pts',(-2.64647562913427,-1.83922289510277,301.303586672688));
#3627=CARTESIAN_POINT('Ctrl Pts',(-2.6586120071956,-1.82163562989948,301.302247773877));
#3628=CARTESIAN_POINT('Ctrl Pts',(-2.68246785346804,-1.78631894103634,301.299600772632));
#3629=CARTESIAN_POINT('Ctrl Pts',(-2.6941886474835,-1.76859173644498,301.298292630756));
#3630=CARTESIAN_POINT('Ctrl Pts',(-2.72498550734598,-1.72099606118296,301.294831142034));
#3631=CARTESIAN_POINT('Ctrl Pts',(-2.74374623397127,-1.69092586774839,301.292696769458));
#3632=CARTESIAN_POINT('Ctrl Pts',(-2.78512765680131,-1.62209581055673,301.287914749298));
#3633=CARTESIAN_POINT('Ctrl Pts',(-2.80744275713907,-1.58316025860629,301.285282137501));
#3634=CARTESIAN_POINT('Ctrl Pts',(-2.88023795856153,-1.4497639774965,301.276462399039));
#3635=CARTESIAN_POINT('Ctrl Pts',(-2.92682278557449,-1.35325428603195,301.270412113192));
#3636=CARTESIAN_POINT('Ctrl Pts',(-3.05778951249449,-1.04337290603943,301.251498066971));
#3637=CARTESIAN_POINT('Ctrl Pts',(-3.12425490059124,-0.823240909377905,
301.238743451911));
#3638=CARTESIAN_POINT('Ctrl Pts',(-3.17711292787648,-0.543288723888024,
301.221963093766));
#3639=CARTESIAN_POINT('Ctrl Pts',(-3.18601280926782,-0.488396394497893,
301.218650368036));
#3640=CARTESIAN_POINT('Ctrl Pts',(-3.19842228888966,-0.396937366890892,
301.213078985377));
#3641=CARTESIAN_POINT('Ctrl Pts',(-3.20273487571026,-0.360490719708634,
301.210845269089));
#3642=CARTESIAN_POINT('Ctrl Pts',(-3.21009463848992,-0.287651167234611,
301.206350558358));
#3643=CARTESIAN_POINT('Ctrl Pts',(-3.213147498771,-0.25126432768427,301.204090091128));
#3644=CARTESIAN_POINT('Ctrl Pts',(-3.2192196670176,-0.160377892211314,301.198403072046));
#3645=CARTESIAN_POINT('Ctrl Pts',(-3.22147382249619,-0.105840337517778,
301.19495381777));
#3646=CARTESIAN_POINT('Ctrl Pts',(-3.22337208614907,0.013456305133541,301.187324709849));
#3647=CARTESIAN_POINT('Ctrl Pts',(-3.22245133808547,0.0781996587369309,
301.183130064313));
#3648=CARTESIAN_POINT('Ctrl Pts',(-3.2132609586872,0.285307921366612,301.169544638267));
#3649=CARTESIAN_POINT('Ctrl Pts',(-3.19749502732674,0.427160833119939,301.159977973014));
#3650=CARTESIAN_POINT('Ctrl Pts',(-3.14226428957243,0.735911014105936,301.138830886301));
#3651=CARTESIAN_POINT('Ctrl Pts',(-3.09877102466537,0.901674028955715,301.127260008606));
#3652=CARTESIAN_POINT('Ctrl Pts',(-3.02973848380263,1.0992071805318,301.113705382374));
#3653=CARTESIAN_POINT('Ctrl Pts',(-3.01651948328793,1.13498114460499,301.111261102602));
#3654=CARTESIAN_POINT('Ctrl Pts',(-2.99474853941737,1.19082920009342,301.107470861951));
#3655=CARTESIAN_POINT('Ctrl Pts',(-2.98662284026428,1.21106443712615,301.106102926268));
#3656=CARTESIAN_POINT('Ctrl Pts',(-2.97031378161113,1.25051578372242,301.103448672512));
#3657=CARTESIAN_POINT('Ctrl Pts',(-2.96214790108208,1.26973758360641,301.102161573342));
#3658=CARTESIAN_POINT('Ctrl Pts',(-2.94035171587583,1.31968911012023,301.098829552937));
#3659=CARTESIAN_POINT('Ctrl Pts',(-2.92642601848393,1.35028830888471,301.096801114455));
#3660=CARTESIAN_POINT('Ctrl Pts',(-2.84072075294001,1.5310531480985,301.084862002645));
#3661=CARTESIAN_POINT('Ctrl Pts',(-2.75786696914208,1.67570882832922,301.075481696633));
#3662=CARTESIAN_POINT('Ctrl Pts',(-2.54295500602276,1.99146429361558,301.054028608583));
#3663=CARTESIAN_POINT('Ctrl Pts',(-2.4041623443193,2.15697574230061,301.042003189011));
#3664=CARTESIAN_POINT('Ctrl Pts',(-2.2090906640932,2.34718653378429,301.025974837117));
#3665=CARTESIAN_POINT('Ctrl Pts',(-2.1672362262738,2.38588615679911,301.022582423097));
#3666=CARTESIAN_POINT('Ctrl Pts',(-2.09658858650008,2.44781528355479,301.016915174149));
#3667=CARTESIAN_POINT('Ctrl Pts',(-2.06838166952625,2.4716958674441,301.014667202694));
#3668=CARTESIAN_POINT('Ctrl Pts',(-2.0116750446927,2.51805441690071,301.01017292876));
#3669=CARTESIAN_POINT('Ctrl Pts',(-1.9831938859128,2.5405464717554,301.007927654445));
#3670=CARTESIAN_POINT('Ctrl Pts',(-1.91193839791788,2.59488973420661,301.002336430517));
#3671=CARTESIAN_POINT('Ctrl Pts',(-1.86874296911706,2.62616837924515,300.998969422062));
#3672=CARTESIAN_POINT('Ctrl Pts',(-1.65413860550772,2.7735914227825,300.982339853672));
#3673=CARTESIAN_POINT('Ctrl Pts',(-1.47260812854855,2.87408866741503,300.968527613011));
#3674=CARTESIAN_POINT('Ctrl Pts',(-1.12317577973019,3.02569687979525,300.942849370896));
#3675=CARTESIAN_POINT('Ctrl Pts',(-0.958274226056778,3.08189617965034,300.93107942795));
#3676=CARTESIAN_POINT('Ctrl Pts',(-0.752520091850376,3.13389477707587,300.917330126871));
#3677=CARTESIAN_POINT('Ctrl Pts',(-0.715240363419869,3.14261268272783,300.914876100239));
#3678=CARTESIAN_POINT('Ctrl Pts',(-0.656466246644875,3.15525694291316,300.91107433019));
#3679=CARTESIAN_POINT('Ctrl Pts',(-0.635073282425498,3.15963230419091,300.909704403945));
#3680=CARTESIAN_POINT('Ctrl Pts',(-0.593156579751613,3.16776231006098,300.907049445366));
#3681=CARTESIAN_POINT('Ctrl Pts',(-0.57263793945248,3.17153568526683,300.905763583054));
#3682=CARTESIAN_POINT('Ctrl Pts',(-0.519074425484693,3.1808492353663,300.902439396346));
#3683=CARTESIAN_POINT('Ctrl Pts',(-0.485976205180451,3.18607398562912,300.900417406232));
#3684=CARTESIAN_POINT('Ctrl Pts',(-0.411605773256444,3.1966278295378,300.895933891364));
#3685=CARTESIAN_POINT('Ctrl Pts',(-0.370299313783368,3.20167573405516,300.893484717169));
#3686=CARTESIAN_POINT('Ctrl Pts',(-0.235498359699913,3.21550535907748,300.885592504093));
#3687=CARTESIAN_POINT('Ctrl Pts',(-0.141712217226645,3.221001982046,300.88025759648));
#3688=CARTESIAN_POINT('Ctrl Pts',(0.210172167162838,3.22622340342791,300.860415233727));
#3689=CARTESIAN_POINT('Ctrl Pts',(0.467663024958985,3.19905803019254,300.846160749087));
#3690=CARTESIAN_POINT('Ctrl Pts',(0.769549770924178,3.12994940917951,300.827854387569));
#3691=CARTESIAN_POINT('Ctrl Pts',(0.819656191181735,3.11720282385432,300.824765123725));
#3692=CARTESIAN_POINT('Ctrl Pts',(0.903762576384387,3.09363893144115,300.819481683605));
#3693=CARTESIAN_POINT('Ctrl Pts',(0.937929671882019,3.08345202787499,300.817307646901));
#3694=CARTESIAN_POINT('Ctrl Pts',(1.00744792827213,3.06146284911055,300.812823945922));
#3695=CARTESIAN_POINT('Ctrl Pts',(1.04277732018905,3.0496100379103,300.810512938629));
#3696=CARTESIAN_POINT('Ctrl Pts',(1.13315022490661,3.01753644349174,300.804514294769));
#3697=CARTESIAN_POINT('Ctrl Pts',(1.18785977209493,2.99642187992722,300.800798388116));
#3698=CARTESIAN_POINT('Ctrl Pts',(1.3078750771396,2.9462998645552,300.792453432364));
#3699=CARTESIAN_POINT('Ctrl Pts',(1.37285243119301,2.91658964956414,300.787804277415));
#3700=CARTESIAN_POINT('Ctrl Pts',(1.59306701486275,2.80690891557254,300.771603948267));
#3701=CARTESIAN_POINT('Ctrl Pts',(1.74275568726422,2.71650413598036,300.75979036805));
#3702=CARTESIAN_POINT('Ctrl Pts',(1.9939557294236,2.53544955282293,300.738942127581));
#3703=CARTESIAN_POINT('Ctrl Pts',(2.09847356513752,2.449648755529,300.729909877036));
#3704=CARTESIAN_POINT('Ctrl Pts',(2.22094805248526,2.3354982089623,300.719132689149));
#3705=CARTESIAN_POINT('Ctrl Pts',(2.24425918410452,2.31310679234612,300.717072293906));
#3706=CARTESIAN_POINT('Ctrl Pts',(2.28045044231943,2.27728113395602,300.713864425716));
#3707=CARTESIAN_POINT('Ctrl Pts',(2.29355727659156,2.26408008880387,300.712700756559));
#3708=CARTESIAN_POINT('Ctrl Pts',(2.32154037620654,2.23540344763261,300.710213618923));
#3709=CARTESIAN_POINT('Ctrl Pts',(2.33637787553941,2.21989116272948,300.708893124301));
#3710=CARTESIAN_POINT('Ctrl Pts',(2.37600815126554,2.17762103131011,300.705357596258));
#3711=CARTESIAN_POINT('Ctrl Pts',(2.4005041380894,2.1505878780608,300.703162994628));
#3712=CARTESIAN_POINT('Ctrl Pts',(2.45527387975482,2.08804322715453,300.698218993814));
#3713=CARTESIAN_POINT('Ctrl Pts',(2.48524634108066,2.05227809008357,300.695486201604));
#3714=CARTESIAN_POINT('Ctrl Pts',(2.58629395556978,1.9262396823475,300.686127443769));
#3715=CARTESIAN_POINT('Ctrl Pts',(2.65331476419022,1.83282277765959,300.679656324057));
#3716=CARTESIAN_POINT('Ctrl Pts',(2.83180430068046,1.55365811498024,300.661046339581));
#3717=CARTESIAN_POINT('Ctrl Pts',(2.92972362144358,1.36002908993869,300.648964795727));
#3718=CARTESIAN_POINT('Ctrl Pts',(3.02770628031384,1.10556583450756,300.632913304538));
#3719=CARTESIAN_POINT('Ctrl Pts',(3.04653891883523,1.05255935604962,300.629563810806));
#3720=CARTESIAN_POINT('Ctrl Pts',(3.0753880828721,0.964085702392131,300.623948239376));
#3721=CARTESIAN_POINT('Ctrl Pts',(3.08620092283184,0.928890088242497,300.621707983677));
#3722=CARTESIAN_POINT('Ctrl Pts',(3.10650185738157,0.858538985392412,300.6172137711));
#3723=CARTESIAN_POINT('Ctrl Pts',(3.11600183482399,0.823392601023137,300.614960576127));
#3724=CARTESIAN_POINT('Ctrl Pts',(3.13810474941508,0.735751411190933,300.60931922431));
#3725=CARTESIAN_POINT('Ctrl Pts',(3.14998755182577,0.683088158279952,300.605909152221));
#3726=CARTESIAN_POINT('Ctrl Pts',(3.20209880960479,0.421723666838208,300.588876913646));
#3727=CARTESIAN_POINT('Ctrl Pts',(3.22292873155932,0.209730132176812,300.574674566188));
#3728=CARTESIAN_POINT('Ctrl Pts',(3.22274884483193,-0.00272866899239652,
300.5603484081));
#3729=CARTESIAN_POINT('Ctrl Pts',(3.22274884385928,-0.00272981751187232,
300.560348330655));
#3730=CARTESIAN_POINT('Ctrl Pts',(3.22263402356394,-0.138283557810964,300.551207902855));
#3731=CARTESIAN_POINT('Ctrl Pts',(3.21396693228134,-0.273703941416887,300.54205285242));
#3732=CARTESIAN_POINT('Ctrl Pts',(3.19035975633614,-0.458589497413305,300.529792771035));
#3733=CARTESIAN_POINT('Ctrl Pts',(3.18273208395242,-0.508838635045151,300.526486096843));
#3734=CARTESIAN_POINT('Ctrl Pts',(3.17007469760743,-0.580719665148035,300.521811256994));
#3735=CARTESIAN_POINT('Ctrl Pts',(3.16600533064313,-0.602510766804593,300.520401429198));
#3736=CARTESIAN_POINT('Ctrl Pts',(3.15763570940016,-0.644900760220875,300.517675528554));
#3737=CARTESIAN_POINT('Ctrl Pts',(3.15335787500929,-0.665503154493343,300.51635838811));
#3738=CARTESIAN_POINT('Ctrl Pts',(3.14427972183635,-0.707169880936442,300.513712214637));
#3739=CARTESIAN_POINT('Ctrl Pts',(3.13946880615948,-0.728230654001299,300.512383782968));
#3740=CARTESIAN_POINT('Ctrl Pts',(3.12581084655722,-0.785368579262997,300.508800632964));
#3741=CARTESIAN_POINT('Ctrl Pts',(3.11655103135972,-0.82134474032904,300.50656730374));
#3742=CARTESIAN_POINT('Ctrl Pts',(3.05664870658941,-1.03845475247073,300.493184028216));
#3743=CARTESIAN_POINT('Ctrl Pts',(2.99084633230843,-1.2150486230341,300.482684704198));
#3744=CARTESIAN_POINT('Ctrl Pts',(2.82517085049119,-1.56317040140482,300.461045708711));
#3745=CARTESIAN_POINT('Ctrl Pts',(2.72414303459175,-1.73324163970284,300.449933952863));
#3746=CARTESIAN_POINT('Ctrl Pts',(2.5775446613667,-1.93522719381413,300.435188088566));
#3747=CARTESIAN_POINT('Ctrl Pts',(2.54587245025847,-1.97670781637585,300.432070924453));
#3748=CARTESIAN_POINT('Ctrl Pts',(2.49061515624663,-2.0455454899615,300.42673287346));
#3749=CARTESIAN_POINT('Ctrl Pts',(2.46755143369191,-2.07330894209824,300.424532399853));
#3750=CARTESIAN_POINT('Ctrl Pts',(2.42263563218952,-2.12556607624192,300.420295341215));
#3751=CARTESIAN_POINT('Ctrl Pts',(2.40086601484393,-2.15012483484957,300.418262248426));
#3752=CARTESIAN_POINT('Ctrl Pts',(2.34212085698658,-2.21439179561324,300.412827036108));
#3753=CARTESIAN_POINT('Ctrl Pts',(2.30451240997127,-2.25350463246978,300.409399021457));
#3754=CARTESIAN_POINT('Ctrl Pts',(2.09525675002074,-2.46041252029592,300.390587583881));
#3755=CARTESIAN_POINT('Ctrl Pts',(1.90628076146895,-2.60955735949895,300.374441273762));
#3756=CARTESIAN_POINT('Ctrl Pts',(1.6160190181811,-2.79015857136675,300.351397885107));
#3757=CARTESIAN_POINT('Ctrl Pts',(1.52698572853849,-2.83986245727343,300.344548760881));
#3758=CARTESIAN_POINT('Ctrl Pts',(1.39668735227513,-2.9047005154241,300.33495352086));
#3759=CARTESIAN_POINT('Ctrl Pts',(1.35723895516576,-2.92334113684662,300.332102468478));
#3760=CARTESIAN_POINT('Ctrl Pts',(1.28574892773296,-2.9553632193987,300.327046142321));
#3761=CARTESIAN_POINT('Ctrl Pts',(1.25384669183796,-2.96903869264591,300.324828360815));
#3762=CARTESIAN_POINT('Ctrl Pts',(1.20220267910952,-2.99019589975931,300.321306764935));
#3763=CARTESIAN_POINT('Ctrl Pts',(1.18259816006196,-2.99800341266394,300.319985603349));
#3764=CARTESIAN_POINT('Ctrl Pts',(1.14283730650054,-3.01338746836862,300.317339642542));
#3765=CARTESIAN_POINT('Ctrl Pts',(1.12267900572573,-3.02095565241521,300.316015318002));
#3766=CARTESIAN_POINT('Ctrl Pts',(1.06786733268022,-3.04090957565896,300.312456821993));
#3767=CARTESIAN_POINT('Ctrl Pts',(1.03307424835159,-3.05290509813842,300.310243541878));
#3768=CARTESIAN_POINT('Ctrl Pts',(0.818982685910732,-3.12263740205925,300.296858473464));
#3769=CARTESIAN_POINT('Ctrl Pts',(0.635093942554579,-3.16516479363169,300.286342352417));
#3770=CARTESIAN_POINT('Ctrl Pts',(0.255463558805834,-3.21851914376431,300.264825495707));
#3771=CARTESIAN_POINT('Ctrl Pts',(0.0603560283042357,-3.22807598171627,
300.253854329408));
#3772=CARTESIAN_POINT('Ctrl Pts',(-0.187820234823062,-3.21771638988053,
300.239195990994));
#3773=CARTESIAN_POINT('Ctrl Pts',(-0.241164486279621,-3.21415843061964,
300.236005987414));
#3774=CARTESIAN_POINT('Ctrl Pts',(-0.330554862086876,-3.20595846777733,
300.230581421172));
#3775=CARTESIAN_POINT('Ctrl Pts',(-0.366656446533083,-3.2020304653081,300.228368927455));
#3776=CARTESIAN_POINT('Ctrl Pts',(-0.439321513808164,-3.19287924149815,
300.223868241477));
#3777=CARTESIAN_POINT('Ctrl Pts',(-0.475876891971064,-3.18763584025664,
300.221579742092));
#3778=CARTESIAN_POINT('Ctrl Pts',(-0.568452387376828,-3.17272918695839,
300.215718983643));
#3779=CARTESIAN_POINT('Ctrl Pts',(-0.624319929774472,-3.16221008112863,
300.212120962107));
#3780=CARTESIAN_POINT('Ctrl Pts',(-0.892317525167407,-3.10437109075683,
300.194555764433));
#3781=CARTESIAN_POINT('Ctrl Pts',(-1.0995463289475,-3.03715696783775,300.179989180362));
#3782=CARTESIAN_POINT('Ctrl Pts',(-1.35828667077545,-2.92326112942877,300.160924389405));
#3783=CARTESIAN_POINT('Ctrl Pts',(-1.41733349196844,-2.8950921639252,300.156514620214));
#3784=CARTESIAN_POINT('Ctrl Pts',(-1.47546414420613,-2.86515673596787,300.152134095017));
#3785=CARTESIAN_POINT('Ctrl Pts',(-1.47546400147781,-2.86515680946839,299.907672586636));
#3786=CARTESIAN_POINT('Ctrl Pts',(-1.46614549632343,-2.86995554120183,299.908379383872));
#3787=CARTESIAN_POINT('Ctrl Pts',(-1.45680248144607,-2.87470937826137,299.909086182415));
#3788=CARTESIAN_POINT('Ctrl Pts',(-1.35630692718034,-2.92522681046287,299.916667929943));
#3789=CARTESIAN_POINT('Ctrl Pts',(-1.2630510708519,-2.96668573293135,299.923523196095));
#3790=CARTESIAN_POINT('Ctrl Pts',(-1.12729366034639,-3.01947552888274,299.933126642353));
#3791=CARTESIAN_POINT('Ctrl Pts',(-1.0862858066101,-3.03446979761809,299.935979874891));
#3792=CARTESIAN_POINT('Ctrl Pts',(-1.01212912733449,-3.05988863794045,299.941040034042));
#3793=CARTESIAN_POINT('Ctrl Pts',(-0.979092601259422,-3.07061911459943,
299.943259483826));
#3794=CARTESIAN_POINT('Ctrl Pts',(-0.92569797176187,-3.08701261292958,299.946783918306));
#3795=CARTESIAN_POINT('Ctrl Pts',(-0.905447115323019,-3.09301296457067,
299.948106271847));
#3796=CARTESIAN_POINT('Ctrl Pts',(-0.864407938164433,-3.10473529840201,
299.950755134605));
#3797=CARTESIAN_POINT('Ctrl Pts',(-0.84361837254559,-3.11044859442196,299.952081159809));
#3798=CARTESIAN_POINT('Ctrl Pts',(-0.787125172449847,-3.1253657141003,299.955645560967));
#3799=CARTESIAN_POINT('Ctrl Pts',(-0.751317393496701,-3.13416644625843,
299.957862956354));
#3800=CARTESIAN_POINT('Ctrl Pts',(-0.532671359600873,-3.18394181369133,
299.971192280551));
#3801=CARTESIAN_POINT('Ctrl Pts',(-0.346678237634265,-3.20952546969058,
299.98165617031));
#3802=CARTESIAN_POINT('Ctrl Pts',(0.0372148264363069,-3.22854829431113,
300.003228977299));
#3803=CARTESIAN_POINT('Ctrl Pts',(0.234388536033836,-3.22024239596763,300.014310004518));
#3804=CARTESIAN_POINT('Ctrl Pts',(0.482051794969479,-3.18693405805876,300.029063880486));
#3805=CARTESIAN_POINT('Ctrl Pts',(0.534357668223951,-3.178582079839,300.03222565744));
#3806=CARTESIAN_POINT('Ctrl Pts',(0.622080479900717,-3.16234845936203,300.037618309369));
#3807=CARTESIAN_POINT('Ctrl Pts',(0.657614014048308,-3.15515063787719,300.039827788519));
#3808=CARTESIAN_POINT('Ctrl Pts',(0.729240404471182,-3.13937919173193,300.044335982624));
#3809=CARTESIAN_POINT('Ctrl Pts',(0.765321674172179,-3.13077879013615,300.046635236049));
#3810=CARTESIAN_POINT('Ctrl Pts',(0.857011999069836,-3.10724360394996,300.052553853443));
#3811=CARTESIAN_POINT('Ctrl Pts',(0.912382047605976,-3.09143829261983,300.056199967282));
#3812=CARTESIAN_POINT('Ctrl Pts',(1.12495959550549,-3.02454992160777,300.070486066516));
#3813=CARTESIAN_POINT('Ctrl Pts',(1.27855345736226,-2.96289134481449,300.081443362004));
#3814=CARTESIAN_POINT('Ctrl Pts',(1.56088046982927,-2.82350041126875,300.10260935198));
#3815=CARTESIAN_POINT('Ctrl Pts',(1.69026189260278,-2.74800263035757,300.112761577617));
#3816=CARTESIAN_POINT('Ctrl Pts',(1.85816883150405,-2.63366485023254,300.126251269833));
#3817=CARTESIAN_POINT('Ctrl Pts',(1.90165112551842,-2.60244221840407,300.129774428926));
#3818=CARTESIAN_POINT('Ctrl Pts',(1.97650701846783,-2.54581317211189,300.135867306005));
#3819=CARTESIAN_POINT('Ctrl Pts',(2.00821843609142,-2.52087360788797,300.138457536914));
#3820=CARTESIAN_POINT('Ctrl Pts',(2.0566934255627,-2.48125480178025,300.142420890205));
#3821=CARTESIAN_POINT('Ctrl Pts',(2.07378616993264,-2.46698687183886,300.143819166602));
#3822=CARTESIAN_POINT('Ctrl Pts',(2.10624022151505,-2.43932061628085,300.146473293157));
#3823=CARTESIAN_POINT('Ctrl Pts',(2.12162452493683,-2.42595184109241,300.147730879588));
#3824=CARTESIAN_POINT('Ctrl Pts',(2.16080206350537,-2.39124928900228,300.150934838974));
#3825=CARTESIAN_POINT('Ctrl Pts',(2.18440742048186,-2.36970528001336,300.152866728992));
#3826=CARTESIAN_POINT('Ctrl Pts',(2.2953856884683,-2.26535047645006,300.161978356271));
#3827=CARTESIAN_POINT('Ctrl Pts',(2.3784016363506,-2.17803109228465,300.168883675901));
#3828=CARTESIAN_POINT('Ctrl Pts',(2.57658716420537,-1.94468965340345,300.186211081492));
#3829=CARTESIAN_POINT('Ctrl Pts',(2.68436472026635,-1.79298789611831,300.196490910727));
#3830=CARTESIAN_POINT('Ctrl Pts',(2.81567899391501,-1.5695416581134,300.211305940885));
#3831=CARTESIAN_POINT('Ctrl Pts',(2.85070593620296,-1.50498636033014,300.215548419476));
#3832=CARTESIAN_POINT('Ctrl Pts',(2.91021508841622,-1.38576510259615,300.223369105823));
#3833=CARTESIAN_POINT('Ctrl Pts',(2.9354368293058,-1.33150544375763,300.226923130811));
#3834=CARTESIAN_POINT('Ctrl Pts',(2.97399257814137,-1.24213243752777,300.23278725562));
#3835=CARTESIAN_POINT('Ctrl Pts',(2.98824927242489,-1.20743155264031,300.235066471179));
#3836=CARTESIAN_POINT('Ctrl Pts',(3.01483452526991,-1.13936604599897,300.239545649583));
#3837=CARTESIAN_POINT('Ctrl Pts',(3.02722290768759,-1.10603051998512,300.241743253915));
#3838=CARTESIAN_POINT('Ctrl Pts',(3.05332859888578,-1.03205677830358,300.246631119012));
#3839=CARTESIAN_POINT('Ctrl Pts',(3.06679122154376,-0.991336498470313,300.249329131737));
#3840=CARTESIAN_POINT('Ctrl Pts',(3.11432475099745,-0.837314530139717,300.259566150404));
#3841=CARTESIAN_POINT('Ctrl Pts',(3.14295773488408,-0.72244431135342,300.267269751636));
#3842=CARTESIAN_POINT('Ctrl Pts',(3.20360838933636,-0.405800018996798,300.288640190842));
#3843=CARTESIAN_POINT('Ctrl Pts',(3.2228735108854,-0.202137207769175,300.302557468846));
#3844=CARTESIAN_POINT('Ctrl Pts',(3.22269570388895,0.0902716330811216,300.322059925417));
#3845=CARTESIAN_POINT('Ctrl Pts',(3.21901202739808,0.178551479280643,300.327878945683));
#3846=CARTESIAN_POINT('Ctrl Pts',(3.20923678664985,0.296324004970847,300.335462112288));
#3847=CARTESIAN_POINT('Ctrl Pts',(3.2063542597418,0.32603861213874,300.337359886027));
#3848=CARTESIAN_POINT('Ctrl Pts',(3.20082595493413,0.375819287096127,300.340508502232));
#3849=CARTESIAN_POINT('Ctrl Pts',(3.19840336453674,0.395907735287083,300.341770578645));
#3850=CARTESIAN_POINT('Ctrl Pts',(3.19279943956598,0.438960905865326,300.344455882313));
#3851=CARTESIAN_POINT('Ctrl Pts',(3.18955928743408,0.46191618620156,300.34587604657));
#3852=CARTESIAN_POINT('Ctrl Pts',(3.17929516344003,0.529366381325593,300.350019999086));
#3853=CARTESIAN_POINT('Ctrl Pts',(3.1715854860556,0.573752946201102,300.352709795304));
#3854=CARTESIAN_POINT('Ctrl Pts',(3.15097474687815,0.67924536015374,300.359044346623));
#3855=CARTESIAN_POINT('Ctrl Pts',(3.13722314816176,0.740167428901892,300.362655603398));
#3856=CARTESIAN_POINT('Ctrl Pts',(3.0686037815018,1.00771075404882,300.378452907558));
#3857=CARTESIAN_POINT('Ctrl Pts',(2.99502943570183,1.20897248037131,300.390206930343));
#3858=CARTESIAN_POINT('Ctrl Pts',(2.85441133976939,1.50015420372206,300.408655573263));
#3859=CARTESIAN_POINT('Ctrl Pts',(2.80175723048675,1.59633328673677,300.415004294568));
#3860=CARTESIAN_POINT('Ctrl Pts',(2.72020783428982,1.7287858037857,300.424249294867));
#3861=CARTESIAN_POINT('Ctrl Pts',(2.69527131926595,1.76741144565827,300.427008958671));
#3862=CARTESIAN_POINT('Ctrl Pts',(2.64973620397425,1.83473769581279,300.431941230587));
#3863=CARTESIAN_POINT('Ctrl Pts',(2.62947563826553,1.86365825170514,300.43410121707));
#3864=CARTESIAN_POINT('Ctrl Pts',(2.58573447791983,1.9239622097851,300.438696381022));
#3865=CARTESIAN_POINT('Ctrl Pts',(2.56214849305656,1.95526168648685,300.441135325997));
#3866=CARTESIAN_POINT('Ctrl Pts',(2.4956523392103,2.04023487135188,300.447910828199));
#3867=CARTESIAN_POINT('Ctrl Pts',(2.45158922512294,2.09297589327371,300.452291211085));
#3868=CARTESIAN_POINT('Ctrl Pts',(2.34647346527397,2.21091630712071,300.462503191567));
#3869=CARTESIAN_POINT('Ctrl Pts',(2.28433028802861,2.27506522200026,300.468372768338));
#3870=CARTESIAN_POINT('Ctrl Pts',(2.11060106485386,2.44009963479235,300.484313929542));
#3871=CARTESIAN_POINT('Ctrl Pts',(1.99448371141188,2.53589325896144,300.494501474038));
#3872=CARTESIAN_POINT('Ctrl Pts',(1.77172163757331,2.69487121418497,300.512901042201));
#3873=CARTESIAN_POINT('Ctrl Pts',(1.66729341278445,2.76070035370338,300.521121186726));
#3874=CARTESIAN_POINT('Ctrl Pts',(1.53127019096326,2.8359051379479,300.531123197489));
#3875=CARTESIAN_POINT('Ctrl Pts',(1.50296868845176,2.85100537518207,300.533167404367));
#3876=CARTESIAN_POINT('Ctrl Pts',(1.4579294875811,2.8741788658863,300.536357412042));
#3877=CARTESIAN_POINT('Ctrl Pts',(1.44133996765233,2.88253390110471,300.537519093158));
#3878=CARTESIAN_POINT('Ctrl Pts',(1.40533108078542,2.90028056584591,300.540010501111));
#3879=CARTESIAN_POINT('Ctrl Pts',(1.38588775254039,2.90962162574655,300.541337129728));
#3880=CARTESIAN_POINT('Ctrl Pts',(1.33291411002999,2.93441997828049,300.544905154062));
#3881=CARTESIAN_POINT('Ctrl Pts',(1.29920865155803,2.94949788421,300.547125496191));
#3882=CARTESIAN_POINT('Ctrl Pts',(1.22164211681965,2.98260896973022,300.552138436531));
#3883=CARTESIAN_POINT('Ctrl Pts',(1.17762673374779,3.00026022397891,300.554913747891));
#3884=CARTESIAN_POINT('Ctrl Pts',(1.02251021525017,3.05852586258049,300.564506150169));
#3885=CARTESIAN_POINT('Ctrl Pts',(0.909572631945766,3.09399227562682,300.571160358045));
#3886=CARTESIAN_POINT('Ctrl Pts',(0.592380749544747,3.17472662156811,300.589537762823));
#3887=CARTESIAN_POINT('Ctrl Pts',(0.385309314099095,3.20645157455163,300.601221245527));
#3888=CARTESIAN_POINT('Ctrl Pts',(0.11924498999209,3.22105594355245,300.616890936495));
#3889=CARTESIAN_POINT('Ctrl Pts',(0.0617867178307858,3.2226701001455,300.620310627769));
#3890=CARTESIAN_POINT('Ctrl Pts',(-0.0327533424388702,3.22279678224083,
300.626012371631));
#3891=CARTESIAN_POINT('Ctrl Pts',(-0.0698219772959573,3.22220679031655,
300.628266918268));
#3892=CARTESIAN_POINT('Ctrl Pts',(-0.143119248527061,3.2197748090424,300.632766185502));
#3893=CARTESIAN_POINT('Ctrl Pts',(-0.179343338382857,3.21796033846117,300.635009732994));
#3894=CARTESIAN_POINT('Ctrl Pts',(-0.26845426016443,3.21198749200961,300.640581159139));
#3895=CARTESIAN_POINT('Ctrl Pts',(-0.321282255254522,3.20713400559933,300.643929705222));
#3896=CARTESIAN_POINT('Ctrl Pts',(-0.571595807127612,3.17789036856934,300.660021811296));
#3897=CARTESIAN_POINT('Ctrl Pts',(-0.76663673476866,3.13655159098987,300.673268880885));
#3898=CARTESIAN_POINT('Ctrl Pts',(-1.13327903897695,3.02258661890292,300.699139630684));
#3899=CARTESIAN_POINT('Ctrl Pts',(-1.30491707642323,2.95255000672305,300.711685762921));
#3900=CARTESIAN_POINT('Ctrl Pts',(-1.50249764822595,2.85131274701742,300.726049926427));
#3901=CARTESIAN_POINT('Ctrl Pts',(-1.53509989300249,2.83389346046958,300.728416553639));
#3902=CARTESIAN_POINT('Ctrl Pts',(-1.58625053171304,2.80542196644905,300.732115667487));
#3903=CARTESIAN_POINT('Ctrl Pts',(-1.60499904813429,2.79473814081267,300.733468486261));
#3904=CARTESIAN_POINT('Ctrl Pts',(-1.64186948007166,2.77323413248643,300.736120744368));
#3905=CARTESIAN_POINT('Ctrl Pts',(-1.65999507255093,2.7624227312071,300.737420548346));
#3906=CARTESIAN_POINT('Ctrl Pts',(-1.70759825673703,2.73339103474394,300.740826968178));
#3907=CARTESIAN_POINT('Ctrl Pts',(-1.73689131474505,2.71487147602817,300.742915708644));
#3908=CARTESIAN_POINT('Ctrl Pts',(-1.80228878018694,2.67203423445684,300.747575270932));
#3909=CARTESIAN_POINT('Ctrl Pts',(-1.83821108902838,2.64745011647853,300.75013220325));
#3910=CARTESIAN_POINT('Ctrl Pts',(-1.95616650442604,2.56316632108192,300.758558001915));
#3911=CARTESIAN_POINT('Ctrl Pts',(-2.03588097144029,2.50031995960859,300.764302624803));
#3912=CARTESIAN_POINT('Ctrl Pts',(-2.29446550456624,2.27587385211834,300.783573153777));
#3913=CARTESIAN_POINT('Ctrl Pts',(-2.45812780828279,2.09804004724571,300.796938039432));
#3914=CARTESIAN_POINT('Ctrl Pts',(-2.63242613205356,1.85994147683927,300.814340667441));
#3915=CARTESIAN_POINT('Ctrl Pts',(-2.66330325905612,1.81545170442136,300.817570297326));
#3916=CARTESIAN_POINT('Ctrl Pts',(-2.71107379633234,1.74277763556684,300.822823996123));
#3917=CARTESIAN_POINT('Ctrl Pts',(-2.72868319503614,1.71507519279603,300.824821661315));
#3918=CARTESIAN_POINT('Ctrl Pts',(-2.76479379020732,1.65630315677302,300.829052232402));
#3919=CARTESIAN_POINT('Ctrl Pts',(-2.78320127632047,1.62518163270348,300.831288123116));
#3920=CARTESIAN_POINT('Ctrl Pts',(-2.82699392869198,1.54821464223496,300.836810342943));
#3921=CARTESIAN_POINT('Ctrl Pts',(-2.85179127982464,1.50204834970549,300.840116509032));
#3922=CARTESIAN_POINT('Ctrl Pts',(-2.9667859886612,1.27483633875973,300.856367389074));
#3923=CARTESIAN_POINT('Ctrl Pts',(-3.04091631812592,1.08620092052891,300.869836813035));
#3924=CARTESIAN_POINT('Ctrl Pts',(-3.1475341004324,0.715997393708384,300.895798573365));
#3925=CARTESIAN_POINT('Ctrl Pts',(-3.18311719071375,0.536094142515357,300.908205531704));
#3926=CARTESIAN_POINT('Ctrl Pts',(-3.20730253177424,0.317331048487601,300.922447022555));
#3927=CARTESIAN_POINT('Ctrl Pts',(-3.2107368651734,0.280459571292043,300.924818082341));
#3928=CARTESIAN_POINT('Ctrl Pts',(-3.21516675256344,0.222005647222841,300.928522451926));
#3929=CARTESIAN_POINT('Ctrl Pts',(-3.21658201609482,0.20045934514703,300.929876185759));
#3930=CARTESIAN_POINT('Ctrl Pts',(-3.2189515384922,0.157839926864977,300.932528664378));
#3931=CARTESIAN_POINT('Ctrl Pts',(-3.21991565688435,0.136768618924221,300.93382779728));
#3932=CARTESIAN_POINT('Ctrl Pts',(-3.22191471378086,0.0811166838642623,
300.937230097217));
#3933=CARTESIAN_POINT('Ctrl Pts',(-3.2225998757072,0.0465252055962028,300.939315468292));
#3934=CARTESIAN_POINT('Ctrl Pts',(-3.22288864827989,-0.0314966424706036,
300.94396607129));
#3935=CARTESIAN_POINT('Ctrl Pts',(-3.2221716767474,-0.0749219005992654,
300.946517494866));
#3936=CARTESIAN_POINT('Ctrl Pts',(-3.21686730992213,-0.219301100887406,
300.954915308994));
#3937=CARTESIAN_POINT('Ctrl Pts',(-3.20840994987354,-0.320056380476534,
300.960638327528));
#3938=CARTESIAN_POINT('Ctrl Pts',(-3.16369942792079,-0.659995996979792,
300.97993641725));
#3939=CARTESIAN_POINT('Ctrl Pts',(-3.10528972744827,-0.895407799953573,
300.993346292929));
#3940=CARTESIAN_POINT('Ctrl Pts',(-3.00229341645686,-1.17271960752348,301.010794604542));
#3941=CARTESIAN_POINT('Ctrl Pts',(-2.98221100881263,-1.22288758315954,301.014017570457));
#3942=CARTESIAN_POINT('Ctrl Pts',(-2.94792424387216,-1.30266512827609,301.01926341952));
#3943=CARTESIAN_POINT('Ctrl Pts',(-2.93451156287154,-1.33260479933907,301.021260057045));
#3944=CARTESIAN_POINT('Ctrl Pts',(-2.9053524022045,-1.39511778270642,301.025490853516));
#3945=CARTESIAN_POINT('Ctrl Pts',(-2.88950986822036,-1.42764097870992,301.027728034196));
#3946=CARTESIAN_POINT('Ctrl Pts',(-2.84933753465936,-1.50670180877295,301.033258582655));
#3947=CARTESIAN_POINT('Ctrl Pts',(-2.82441200657364,-1.55292338453925,301.036571927484));
#3948=CARTESIAN_POINT('Ctrl Pts',(-2.6984941959091,-1.77335604916429,301.052773858881));
#3949=CARTESIAN_POINT('Ctrl Pts',(-2.58246675679837,-1.93842875697878,301.066181520913));
#3950=CARTESIAN_POINT('Ctrl Pts',(-2.33256375633524,-2.23137379503876,301.092129107037));
#3951=CARTESIAN_POINT('Ctrl Pts',(-2.20156222920794,-2.3607234626445,301.104585821404));
#3952=CARTESIAN_POINT('Ctrl Pts',(-2.0317909080027,-2.50186175628897,301.118870968421));
#3953=CARTESIAN_POINT('Ctrl Pts',(-2.00293249205562,-2.52502440325386,301.121240256945));
#3954=CARTESIAN_POINT('Ctrl Pts',(-1.95661584113431,-2.56090569265645,301.12494252647));
#3955=CARTESIAN_POINT('Ctrl Pts',(-1.93941849782901,-2.57395405316969,301.126295894764));
#3956=CARTESIAN_POINT('Ctrl Pts',(-1.9051566948386,-2.59941159004449,301.128948284674));
#3957=CARTESIAN_POINT('Ctrl Pts',(-1.88809905231737,-2.61182783853808,301.130247685034));
#3958=CARTESIAN_POINT('Ctrl Pts',(-1.842733441423,-2.64417272576674,301.133651627648));
#3959=CARTESIAN_POINT('Ctrl Pts',(-1.81422333950115,-2.66381490141667,301.135738342283));
#3960=CARTESIAN_POINT('Ctrl Pts',(-1.74921659064302,-2.707073695116,301.140392517317));
#3961=CARTESIAN_POINT('Ctrl Pts',(-1.71254714705836,-2.73041924794202,301.142946137042));
#3962=CARTESIAN_POINT('Ctrl Pts',(-1.61011183487701,-2.79275874012439,301.149915900342));
#3963=CARTESIAN_POINT('Ctrl Pts',(-1.54341903546483,-2.83016214338351,301.154272772181));
#3964=CARTESIAN_POINT('Ctrl Pts',(-1.47546399521001,-2.86515681269611,301.158594111703));
#3965=CARTESIAN_POINT('Origin',(0.,0.,294.689226550727));
#3966=CARTESIAN_POINT('',(-1.47546411936631,-2.86515674875958,302.651619072379));
#3967=CARTESIAN_POINT('',(-1.47546400229876,-2.86515680904563,302.404343180173));
#3968=CARTESIAN_POINT('',(-1.47546400239267,-2.86515680899727,294.689226550727));
#3969=CARTESIAN_POINT('Ctrl Pts',(-1.47546411936631,-2.86515674875959,302.651619072379));
#3970=CARTESIAN_POINT('Ctrl Pts',(-1.56656438462051,-2.81824302485756,302.64575923233));
#3971=CARTESIAN_POINT('Ctrl Pts',(-1.65541897282013,-2.76698859902053,302.640007807061));
#3972=CARTESIAN_POINT('Ctrl Pts',(-1.91531531524237,-2.60004896160934,302.622671394209));
#3973=CARTESIAN_POINT('Ctrl Pts',(-2.07778607985001,-2.47214113131752,302.611090056498));
#3974=CARTESIAN_POINT('Ctrl Pts',(-2.26472861339141,-2.29343823920053,302.595812134333));
#3975=CARTESIAN_POINT('Ctrl Pts',(-2.30165889047301,-2.25637331781722,302.592687368049));
#3976=CARTESIAN_POINT('Ctrl Pts',(-2.36252943902848,-2.19223094090484,302.587340313719));
#3977=CARTESIAN_POINT('Ctrl Pts',(-2.38694675230375,-2.16561928537802,302.585138610119));
#3978=CARTESIAN_POINT('Ctrl Pts',(-2.43267313848977,-2.11407058303965,302.580901855647));
#3979=CARTESIAN_POINT('Ctrl Pts',(-2.4540589104674,-2.08920744993729,302.578870341943));
#3980=CARTESIAN_POINT('Ctrl Pts',(-2.50971667940753,-2.02246576596436,302.573445936145));
#3981=CARTESIAN_POINT('Ctrl Pts',(-2.54331852224081,-1.98004442556283,302.570027342711));
#3982=CARTESIAN_POINT('Ctrl Pts',(-2.72072706728567,-1.74410094828758,302.551159292584));
#3983=CARTESIAN_POINT('Ctrl Pts',(-2.84351759392912,-1.53577877699471,302.534938617956));
#3984=CARTESIAN_POINT('Ctrl Pts',(-2.98332211902242,-1.22318859500695,302.511857830567));
#3985=CARTESIAN_POINT('Ctrl Pts',(-3.02033385479007,-1.12871009162387,302.505043086966));
#3986=CARTESIAN_POINT('Ctrl Pts',(-3.06676937987678,-0.991431085146797,
302.495489658053));
#3987=CARTESIAN_POINT('Ctrl Pts',(-3.07987334170464,-0.949942399395154,
302.492646856339));
#3988=CARTESIAN_POINT('Ctrl Pts',(-3.10189393394382,-0.874969193126422,
302.487603449932));
#3989=CARTESIAN_POINT('Ctrl Pts',(-3.11111821030993,-0.841582300140183,
302.485390425793));
#3990=CARTESIAN_POINT('Ctrl Pts',(-3.12508986566979,-0.787639204586613,
302.481874467981));
#3991=CARTESIAN_POINT('Ctrl Pts',(-3.13017660022288,-0.767174495895574,
302.480554280439));
#3992=CARTESIAN_POINT('Ctrl Pts',(-3.14005460400588,-0.725698943893595,
302.477908284888));
#3993=CARTESIAN_POINT('Ctrl Pts',(-3.14483671463996,-0.70468714461658,302.476582981906));
#3994=CARTESIAN_POINT('Ctrl Pts',(-3.15723122900629,-0.647586843247663,
302.473018615286));
#3995=CARTESIAN_POINT('Ctrl Pts',(-3.16443569996564,-0.611412061202154,
302.470800561102));
#3996=CARTESIAN_POINT('Ctrl Pts',(-3.20435211868759,-0.391326344860414,
302.457505079968));
#3997=CARTESIAN_POINT('Ctrl Pts',(-3.22164780622963,-0.204961933966709,
302.447071438326));
#3998=CARTESIAN_POINT('Ctrl Pts',(-3.22379022441715,0.175815524642427,302.425699773419));
#3999=CARTESIAN_POINT('Ctrl Pts',(-3.20737182576775,0.369447017497268,302.414790748178));
#4000=CARTESIAN_POINT('Ctrl Pts',(-3.16415676457459,0.61417357292202,302.400140325852));
#4001=CARTESIAN_POINT('Ctrl Pts',(-3.15330078481984,0.667675715121783,302.396885718481));
#4002=CARTESIAN_POINT('Ctrl Pts',(-3.13292411498144,0.756463732439752,302.391384007003));
#4003=CARTESIAN_POINT('Ctrl Pts',(-3.12415238958639,0.79191070801318,302.389160470346));
#4004=CARTESIAN_POINT('Ctrl Pts',(-3.10536110910862,0.862668348410636,302.384663819488));
#4005=CARTESIAN_POINT('Ctrl Pts',(-3.09533685573578,0.897972089385883,302.382390847854));
#4006=CARTESIAN_POINT('Ctrl Pts',(-3.06861588434326,0.986308681147351,302.376625948904));
#4007=CARTESIAN_POINT('Ctrl Pts',(-3.05114613632413,1.03909331470047,302.373109960628));
#4008=CARTESIAN_POINT('Ctrl Pts',(-2.95462849305133,1.30725639273526,302.354869912481));
#4009=CARTESIAN_POINT('Ctrl Pts',(-2.8541196202872,1.51417295134879,302.339462691277));
#4010=CARTESIAN_POINT('Ctrl Pts',(-2.67576667315583,1.79940280879597,302.316779962849));
#4011=CARTESIAN_POINT('Ctrl Pts',(-2.61451986611871,1.88729054299005,302.309574931153));
#4012=CARTESIAN_POINT('Ctrl Pts',(-2.52156037207488,2.00745194194057,302.299548616362));
#4013=CARTESIAN_POINT('Ctrl Pts',(-2.49337163801645,2.0423585012062,302.296613850176));
#4014=CARTESIAN_POINT('Ctrl Pts',(-2.4416299200101,2.10376243584213,302.291426720655));
#4015=CARTESIAN_POINT('Ctrl Pts',(-2.4183513724015,2.13048114905897,302.289160939516));
#4016=CARTESIAN_POINT('Ctrl Pts',(-2.38041491842719,2.17260072413725,302.285582393459));
#4017=CARTESIAN_POINT('Ctrl Pts',(-2.36603768715614,2.18824925812226,302.284251333726));
#4018=CARTESIAN_POINT('Ctrl Pts',(-2.33689435565397,2.21934651106358,302.281605160707));
#4019=CARTESIAN_POINT('Ctrl Pts',(-2.32212729530856,2.23479284252099,302.280290225134));
#4020=CARTESIAN_POINT('Ctrl Pts',(-2.28206572295433,2.27587132439407,302.276788004346));
#4021=CARTESIAN_POINT('Ctrl Pts',(-2.25649275148975,2.30122900869434,302.274620491556));
#4022=CARTESIAN_POINT('Ctrl Pts',(-2.0882200306413,2.46258210535103,302.260748662559));
#4023=CARTESIAN_POINT('Ctrl Pts',(-1.93370768469685,2.58568475220007,302.249771553372));
#4024=CARTESIAN_POINT('Ctrl Pts',(-1.66145228858582,2.76445584120435,302.231486883426));
#4025=CARTESIAN_POINT('Ctrl Pts',(-1.54988579555216,2.82851398050596,302.224252481611));
#4026=CARTESIAN_POINT('Ctrl Pts',(-1.37991781639501,2.91302260255444,302.213305399926));
#4027=CARTESIAN_POINT('Ctrl Pts',(-1.32427353579774,2.93873660972428,302.209733657307));
#4028=CARTESIAN_POINT('Ctrl Pts',(-1.21973264267542,2.98347423135796,302.203016785893));
#4029=CARTESIAN_POINT('Ctrl Pts',(-1.17103919381826,3.00292073834523,302.199885701727));
#4030=CARTESIAN_POINT('Ctrl Pts',(-1.08802130321314,3.03374897795421,302.194531160167));
#4031=CARTESIAN_POINT('Ctrl Pts',(-1.05393953784335,3.0457568036242,302.19232842976));
#4032=CARTESIAN_POINT('Ctrl Pts',(-0.988572549668914,3.06755865422687,302.188091905358));
#4033=CARTESIAN_POINT('Ctrl Pts',(-0.957325554598902,3.07745340207265,302.186061685676));
#4034=CARTESIAN_POINT('Ctrl Pts',(-0.874217056372091,3.10238253447798,302.180646149307));
#4035=CARTESIAN_POINT('Ctrl Pts',(-0.822121093078396,3.11659256418156,302.17723529002));
#4036=CARTESIAN_POINT('Ctrl Pts',(-0.534734637313234,3.18727506797976,302.158321240372));
#4037=CARTESIAN_POINT('Ctrl Pts',(-0.294046051273407,3.21841030503454,302.142040006514));
#4038=CARTESIAN_POINT('Ctrl Pts',(0.0488040166192698,3.22396307333619,302.118928632269));
#4039=CARTESIAN_POINT('Ctrl Pts',(0.149822360850706,3.22085001862124,302.112141712529));
#4040=CARTESIAN_POINT('Ctrl Pts',(0.293803765892632,3.20962315128552,302.102622143149));
#4041=CARTESIAN_POINT('Ctrl Pts',(0.337005318291248,3.20537504464777,302.099786040111));
#4042=CARTESIAN_POINT('Ctrl Pts',(0.414443646400678,3.19617732247638,302.094753126921));
#4043=CARTESIAN_POINT('Ctrl Pts',(0.448711350365809,3.19154685941951,302.092543968812));
#4044=CARTESIAN_POINT('Ctrl Pts',(0.503735729571337,3.18320781614914,302.089032591804));
#4045=CARTESIAN_POINT('Ctrl Pts',(0.524541397496784,3.17984560624032,302.087713194817));
#4046=CARTESIAN_POINT('Ctrl Pts',(0.566564256985201,3.17263099243986,302.085067163379));
#4047=CARTESIAN_POINT('Ctrl Pts',(0.587778634801142,3.16876928921676,302.08374105874));
#4048=CARTESIAN_POINT('Ctrl Pts',(0.645235979904885,3.15771329676716,302.080171880853));
#4049=CARTESIAN_POINT('Ctrl Pts',(0.681397589133606,3.15010798481078,302.077949914051));
#4050=CARTESIAN_POINT('Ctrl Pts',(0.897744417873805,3.1007070259585,302.064760139779));
#4051=CARTESIAN_POINT('Ctrl Pts',(1.07420751899143,3.04407984601912,302.054422639236));
#4052=CARTESIAN_POINT('Ctrl Pts',(1.43026140794561,2.89497410757814,302.032757840055));
#4053=CARTESIAN_POINT('Ctrl Pts',(1.60798110297047,2.80016234396717,302.021455452306));
#4054=CARTESIAN_POINT('Ctrl Pts',(1.81920805949189,2.66069861594447,302.006499871361));
#4055=CARTESIAN_POINT('Ctrl Pts',(1.86200579665291,2.63092551290022,302.003385827147));
#4056=CARTESIAN_POINT('Ctrl Pts',(1.93317278980825,2.57881028805522,301.998051469096));
#4057=CARTESIAN_POINT('Ctrl Pts',(1.96192358729006,2.5570051259342,301.995851498389));
#4058=CARTESIAN_POINT('Ctrl Pts',(2.0161201967694,2.514449151445,301.991614305894));
#4059=CARTESIAN_POINT('Ctrl Pts',(2.04162699176136,2.49378312715198,301.989580557835));
#4060=CARTESIAN_POINT('Ctrl Pts',(2.10848674787075,2.43789893586445,301.984140866892));
#4061=CARTESIAN_POINT('Ctrl Pts',(2.14927120629997,2.4020200478917,301.98070894846));
#4062=CARTESIAN_POINT('Ctrl Pts',(2.36495365537342,2.20238765548299,301.961921166423));
#4063=CARTESIAN_POINT('Ctrl Pts',(2.52205919402392,2.02056925855705,301.94580587386));
#4064=CARTESIAN_POINT('Ctrl Pts',(2.71531123660843,1.73885874569804,301.92277803093));
#4065=CARTESIAN_POINT('Ctrl Pts',(2.76904364975881,1.65195157013254,301.915914495822));
#4066=CARTESIAN_POINT('Ctrl Pts',(2.83973796607326,1.52443870867897,301.906301739341));
#4067=CARTESIAN_POINT('Ctrl Pts',(2.86013738222023,1.4858127700909,301.903447237298));
#4068=CARTESIAN_POINT('Ctrl Pts',(2.89534016064232,1.41574344741609,301.898385510776));
#4069=CARTESIAN_POINT('Ctrl Pts',(2.91043202295578,1.38445289422434,301.89616574158));
#4070=CARTESIAN_POINT('Ctrl Pts',(2.93387639192436,1.33376623706746,301.892641789615));
#4071=CARTESIAN_POINT('Ctrl Pts',(2.94254903237091,1.31452208804738,301.891320220605));
#4072=CARTESIAN_POINT('Ctrl Pts',(2.95968256914594,1.27548419470277,301.888674270965));
#4073=CARTESIAN_POINT('Ctrl Pts',(2.96813544250033,1.25568821610776,301.887350352388));
#4074=CARTESIAN_POINT('Ctrl Pts',(2.99048739567302,1.20185452999884,301.883794292138));
#4075=CARTESIAN_POINT('Ctrl Pts',(3.00400379852611,1.16766031279254,301.881582992887));
#4076=CARTESIAN_POINT('Ctrl Pts',(3.08335823294515,0.956401588420554,301.868167115089));
#4077=CARTESIAN_POINT('Ctrl Pts',(3.13411434422543,0.774044499453227,301.857622396741));
#4078=CARTESIAN_POINT('Ctrl Pts',(3.20455820707267,0.394614957239556,301.835962098765));
#4079=CARTESIAN_POINT('Ctrl Pts',(3.22267989304969,0.198086985339928,301.824875396434));
#4080=CARTESIAN_POINT('Ctrl Pts',(3.2227683696409,-0.0511815540635796,301.810149796668));
#4081=CARTESIAN_POINT('Ctrl Pts',(3.22151258882781,-0.103497361171781,301.807024556326));
#4082=CARTESIAN_POINT('Ctrl Pts',(3.21725571438089,-0.191472727016841,301.801698658033));
#4083=CARTESIAN_POINT('Ctrl Pts',(3.21493332152809,-0.227155714872538,301.79951894891));
#4084=CARTESIAN_POINT('Ctrl Pts',(3.2089920367645,-0.299774134902215,301.795039839523));
#4085=CARTESIAN_POINT('Ctrl Pts',(3.20532792537239,-0.336700364262504,301.792739368845));
#4086=CARTESIAN_POINT('Ctrl Pts',(3.19432777379486,-0.430961944822834,301.786805157277));
#4087=CARTESIAN_POINT('Ctrl Pts',(3.18608559544938,-0.488176230768828,301.783144327156));
#4088=CARTESIAN_POINT('Ctrl Pts',(3.14761330287636,-0.712340654620758,301.768561188446));
#4089=CARTESIAN_POINT('Ctrl Pts',(3.10576228328249,-0.876998414390794,301.757302235601));
#4090=CARTESIAN_POINT('Ctrl Pts',(2.9840092915615,-1.23503121957962,301.731865741436));
#4091=CARTESIAN_POINT('Ctrl Pts',(2.89785219803998,-1.4255089947519,301.717661870415));
#4092=CARTESIAN_POINT('Ctrl Pts',(2.77659228961666,-1.63641589213254,301.701958606608));
#4093=CARTESIAN_POINT('Ctrl Pts',(2.75881057115451,-1.66621912379549,301.699741156993));
#4094=CARTESIAN_POINT('Ctrl Pts',(2.72944803908689,-1.71367329428893,301.69621995445));
#4095=CARTESIAN_POINT('Ctrl Pts',(2.71816955541944,-1.73150717457507,301.694898860826));
#4096=CARTESIAN_POINT('Ctrl Pts',(2.69502918049024,-1.76731403851098,301.692252897774));
#4097=CARTESIAN_POINT('Ctrl Pts',(2.68316075152255,-1.7852813884695,301.69092850514));
#4098=CARTESIAN_POINT('Ctrl Pts',(2.65052081746639,-1.83363341619955,301.687369600883));
#4099=CARTESIAN_POINT('Ctrl Pts',(2.62940687895751,-1.8637842759102,301.685155988814));
#4100=CARTESIAN_POINT('Ctrl Pts',(2.58003224384247,-1.93178192756879,301.680160560483));
#4101=CARTESIAN_POINT('Ctrl Pts',(2.55144649945041,-1.96938288788776,301.677395867025));
#4102=CARTESIAN_POINT('Ctrl Pts',(2.44891702201815,-2.0982659926791,301.667860058194));
#4103=CARTESIAN_POINT('Ctrl Pts',(2.37081574605065,-2.18612680372307,301.661249907815));
#4104=CARTESIAN_POINT('Ctrl Pts',(2.13991237667403,-2.41891817201873,301.642838775936));
#4105=CARTESIAN_POINT('Ctrl Pts',(1.97747714127827,-2.55342223537591,301.631081348385));
#4106=CARTESIAN_POINT('Ctrl Pts',(1.75555322046565,-2.70322791916428,301.615334616756));
#4107=CARTESIAN_POINT('Ctrl Pts',(1.70716094770546,-2.73404630690465,301.611921168019));
#4108=CARTESIAN_POINT('Ctrl Pts',(1.62622434022472,-2.78260360629044,301.606228559067));
#4109=CARTESIAN_POINT('Ctrl Pts',(1.59414976631164,-2.80110242310004,301.603976777764));
#4110=CARTESIAN_POINT('Ctrl Pts',(1.53006749377038,-2.83660432526885,301.59948223923));
#4111=CARTESIAN_POINT('Ctrl Pts',(1.4980775519221,-2.8536282370309,301.597240637826));
#4112=CARTESIAN_POINT('Ctrl Pts',(1.4185909733147,-2.89422324797366,301.591672818702));
#4113=CARTESIAN_POINT('Ctrl Pts',(1.3707880605459,-2.91716782707154,301.58832593936));
#4114=CARTESIAN_POINT('Ctrl Pts',(1.14094417933643,-3.02059196120465,301.572232368835));
#4115=CARTESIAN_POINT('Ctrl Pts',(0.952295632917648,-3.08526193892359,301.55898181711));
#4116=CARTESIAN_POINT('Ctrl Pts',(0.579113941289261,-3.17568448021665,301.533108715446));
#4117=CARTESIAN_POINT('Ctrl Pts',(0.395881850157772,-3.20369026392042,301.520563825996));
#4118=CARTESIAN_POINT('Ctrl Pts',(0.17438515354406,-3.21824054881868,301.506201888283));
#4119=CARTESIAN_POINT('Ctrl Pts',(0.137480016494186,-3.22002824818947,301.503836268437));
#4120=CARTESIAN_POINT('Ctrl Pts',(0.079000232393424,-3.22185372047421,301.500139196589));
#4121=CARTESIAN_POINT('Ctrl Pts',(0.0574429559807811,-3.22231016516788,
301.498787422204));
#4122=CARTESIAN_POINT('Ctrl Pts',(0.0148080076377847,-3.22278489118032,
301.496137951778));
#4123=CARTESIAN_POINT('Ctrl Pts',(-0.00626830765275662,-3.22281282164261,
301.494839880365));
#4124=CARTESIAN_POINT('Ctrl Pts',(-0.061921713059651,-3.22234060509785,
301.491439573036));
#4125=CARTESIAN_POINT('Ctrl Pts',(-0.0964941240447321,-3.22149070648021,
301.489355124637));
#4126=CARTESIAN_POINT('Ctrl Pts',(-0.174421625000267,-3.21831929344846,
301.484706299137));
#4127=CARTESIAN_POINT('Ctrl Pts',(-0.217757399199872,-3.21567784775963,
301.482155726233));
#4128=CARTESIAN_POINT('Ctrl Pts',(-0.361726871689196,-3.20397852348821,
301.473759695828));
#4129=CARTESIAN_POINT('Ctrl Pts',(-0.461990600573863,-3.19106434030277,
301.468037600735));
#4130=CARTESIAN_POINT('Ctrl Pts',(-0.799674924297983,-3.13131717494294,
301.448735910623));
#4131=CARTESIAN_POINT('Ctrl Pts',(-1.03234034105093,-3.06249755699573,301.435321826378));
#4132=CARTESIAN_POINT('Ctrl Pts',(-1.30484839411577,-2.9472706346054,301.417870478235));
#4133=CARTESIAN_POINT('Ctrl Pts',(-1.35404585412848,-2.92499450542626,301.414649420727));
#4134=CARTESIAN_POINT('Ctrl Pts',(-1.42707972997024,-2.88968800765593,301.409748711068));
#4135=CARTESIAN_POINT('Ctrl Pts',(-1.45135013935263,-2.87757467623773,301.408099925956));
#4136=CARTESIAN_POINT('Ctrl Pts',(-1.47546400249216,-2.86515680894603,301.40644069294));
#4137=CARTESIAN_POINT('',(3.22274880669402,-0.00279346863476049,301.56427538288));
#4138=CARTESIAN_POINT('Ctrl Pts',(-1.47546399521001,-2.86515681269611,301.158594111703));
#4139=CARTESIAN_POINT('Ctrl Pts',(-1.45345302210279,-2.87649175889358,301.159993814913));
#4140=CARTESIAN_POINT('Ctrl Pts',(-1.43130962004888,-2.88757399582668,301.161389750391));
#4141=CARTESIAN_POINT('Ctrl Pts',(-1.19187476928135,-3.00397362883705,301.176373801413));
#4142=CARTESIAN_POINT('Ctrl Pts',(-0.963554646627904,-3.08479757827593,
301.189765730589));
#4143=CARTESIAN_POINT('Ctrl Pts',(-0.67567640453847,-3.15158745199416,301.207195819349));
#4144=CARTESIAN_POINT('Ctrl Pts',(-0.622700029955293,-3.16248102737201,
301.210421449546));
#4145=CARTESIAN_POINT('Ctrl Pts',(-0.537179844503203,-3.17783449708863,
301.215670436555));
#4146=CARTESIAN_POINT('Ctrl Pts',(-0.504797159632848,-3.18313901417946,
301.217667484575));
#4147=CARTESIAN_POINT('Ctrl Pts',(-0.436562901552625,-3.19324889349919,
301.221898188511));
#4148=CARTESIAN_POINT('Ctrl Pts',(-0.400700296424094,-3.19794696163251,
301.224134851375));
#4149=CARTESIAN_POINT('Ctrl Pts',(-0.312639634462214,-3.20797858158073,
301.229662058633));
#4150=CARTESIAN_POINT('Ctrl Pts',(-0.260377280503483,-3.21264272649583,
301.232972523859));
#4151=CARTESIAN_POINT('Ctrl Pts',(-0.00891327128532342,-3.22890850617758,
301.249054300625));
#4152=CARTESIAN_POINT('Ctrl Pts',(0.190937645520774,-3.22326711999056,301.262334276149));
#4153=CARTESIAN_POINT('Ctrl Pts',(0.573394765673103,-3.17676829414263,301.288293177993));
#4154=CARTESIAN_POINT('Ctrl Pts',(0.755561025127526,-3.13843508525341,301.300893813444));
#4155=CARTESIAN_POINT('Ctrl Pts',(0.968768863344022,-3.07391746421563,301.315306053339));
#4156=CARTESIAN_POINT('Ctrl Pts',(1.00393506550612,-3.06261266465628,301.317671001378));
#4157=CARTESIAN_POINT('Ctrl Pts',(1.05932161465258,-3.04375108223454,301.321368124114));
#4158=CARTESIAN_POINT('Ctrl Pts',(1.0796727843825,-3.03659178579029,301.322720596174));
#4159=CARTESIAN_POINT('Ctrl Pts',(1.11979215424178,-3.02202393484573,301.325372772496));
#4160=CARTESIAN_POINT('Ctrl Pts',(1.13956234063291,-3.01462449521813,301.326672832493));
#4161=CARTESIAN_POINT('Ctrl Pts',(1.1916124558994,-2.99455833836158,301.33008082218));
#4162=CARTESIAN_POINT('Ctrl Pts',(1.2237640766479,-2.9815636145052,301.332170846201));
#4163=CARTESIAN_POINT('Ctrl Pts',(1.29581865757841,-2.95107930363049,301.336833822585));
#4164=CARTESIAN_POINT('Ctrl Pts',(1.33558973665409,-2.93329429745238,301.339392854454));
#4165=CARTESIAN_POINT('Ctrl Pts',(1.46687736253742,-2.87136042617462,301.347829335986));
#4166=CARTESIAN_POINT('Ctrl Pts',(1.55666905542917,-2.82368971380537,301.353582208836));
#4167=CARTESIAN_POINT('Ctrl Pts',(1.85101869968063,-2.64910286229942,301.37284228792));
#4168=CARTESIAN_POINT('Ctrl Pts',(2.04355862119677,-2.50357244306358,301.386190049781));
#4169=CARTESIAN_POINT('Ctrl Pts',(2.25742016995655,-2.30067568172881,301.403575289066));
#4170=CARTESIAN_POINT('Ctrl Pts',(2.29578594176301,-2.26239272176716,301.406807441956));
#4171=CARTESIAN_POINT('Ctrl Pts',(2.35581519136251,-2.1993931589936,301.412064113639));
#4172=CARTESIAN_POINT('Ctrl Pts',(2.37809841184491,-2.17528005250291,301.414062168775));
#4173=CARTESIAN_POINT('Ctrl Pts',(2.4241344834076,-2.1239106258541,301.418292659971));
#4174=CARTESIAN_POINT('Ctrl Pts',(2.44780475724229,-2.09658676068211,301.420528066935));
#4175=CARTESIAN_POINT('Ctrl Pts',(2.50462148480605,-2.02872624173379,301.426047158583));
#4176=CARTESIAN_POINT('Ctrl Pts',(2.53724832293572,-1.98776995455119,301.429350627678));
#4177=CARTESIAN_POINT('Ctrl Pts',(2.68811908316454,-1.78861355191994,301.445294303723));
#4178=CARTESIAN_POINT('Ctrl Pts',(2.79263630709289,-1.62058143652535,301.458431928333));
#4179=CARTESIAN_POINT('Ctrl Pts',(2.96547294622877,-1.27574936145966,301.48441684266));
#4180=CARTESIAN_POINT('Ctrl Pts',(3.03493041119149,-1.10035112917256,301.497192056638));
#4181=CARTESIAN_POINT('Ctrl Pts',(3.09918741784172,-0.884596233552232,301.511755564093));
#4182=CARTESIAN_POINT('Ctrl Pts',(3.10909165297782,-0.849130437892967,301.514112857249));
#4183=CARTESIAN_POINT('Ctrl Pts',(3.12382578344141,-0.792650226447109,301.517800901707));
#4184=CARTESIAN_POINT('Ctrl Pts',(3.12905610741522,-0.771744675550877,301.519151792119));
#4185=CARTESIAN_POINT('Ctrl Pts',(3.13899883674654,-0.730239893023231,301.521803605958));
#4186=CARTESIAN_POINT('Ctrl Pts',(3.14371909013409,-0.709643802145879,301.523104844375));
#4187=CARTESIAN_POINT('Ctrl Pts',(3.15567145248582,-0.655030244662248,301.526520049407));
#4188=CARTESIAN_POINT('Ctrl Pts',(3.16255631306451,-0.620938581176801,301.528615971018));
#4189=CARTESIAN_POINT('Ctrl Pts',(3.2045479384828,-0.394148823274494,301.542360648955));
#4190=CARTESIAN_POINT('Ctrl Pts',(3.22257899414355,-0.198690636089394,301.553279316752));
#4191=CARTESIAN_POINT('Ctrl Pts',(3.22274878942769,-0.00279333892986146,
301.564275417346));
#4192=CARTESIAN_POINT('Ctrl Pts',(3.22274878931396,-0.00279347014087786,
301.564275409981));
#4193=CARTESIAN_POINT('Ctrl Pts',(3.22287158591405,0.138873551275113,301.572227458523));
#4194=CARTESIAN_POINT('Ctrl Pts',(3.21365306475287,0.280392099962546,301.580196534937));
#4195=CARTESIAN_POINT('Ctrl Pts',(3.18615340785927,0.48917779355849,301.59238269485));
#4196=CARTESIAN_POINT('Ctrl Pts',(3.17496313149674,0.557204328551994,301.596420487291));
#4197=CARTESIAN_POINT('Ctrl Pts',(3.15461619497305,0.660160745287787,301.602666014397));
#4198=CARTESIAN_POINT('Ctrl Pts',(3.14703931863876,0.695384011309783,301.604826884526));
#4199=CARTESIAN_POINT('Ctrl Pts',(3.13070004798135,0.765594666178743,301.609187089066));
#4200=CARTESIAN_POINT('Ctrl Pts',(3.12193767200957,0.8005766640351,301.611386142309));
#4201=CARTESIAN_POINT('Ctrl Pts',(3.10405568489855,0.867202336719626,301.615628739179));
#4202=CARTESIAN_POINT('Ctrl Pts',(3.09503442337277,0.898867832612129,301.617668921201));
#4203=CARTESIAN_POINT('Ctrl Pts',(3.06971960605143,0.982821590140605,301.623143998793));
#4204=CARTESIAN_POINT('Ctrl Pts',(3.05257624269807,1.03484030065757,301.626605459846));
#4205=CARTESIAN_POINT('Ctrl Pts',(2.95360986286981,1.31123668505557,301.64538058451));
#4206=CARTESIAN_POINT('Ctrl Pts',(2.84837063316787,1.52640217195652,301.661446270562));
#4207=CARTESIAN_POINT('Ctrl Pts',(2.6656750606014,1.8140277932332,301.684414546406));
#4208=CARTESIAN_POINT('Ctrl Pts',(2.60693032213581,1.89748162865093,301.691269811311));
#4209=CARTESIAN_POINT('Ctrl Pts',(2.51752931484781,2.01247847508349,301.700873254601));
#4210=CARTESIAN_POINT('Ctrl Pts',(2.49003558251926,2.04639844646671,301.703726485868));
#4211=CARTESIAN_POINT('Ctrl Pts',(2.43944647981816,2.10628220260853,301.708786642058));
#4212=CARTESIAN_POINT('Ctrl Pts',(2.41660452503261,2.13245085202524,301.711006090195));
#4213=CARTESIAN_POINT('Ctrl Pts',(2.37919927561547,2.17393063652948,301.714530520455));
#4214=CARTESIAN_POINT('Ctrl Pts',(2.36490119351079,2.1894761978161,301.71585287147));
#4215=CARTESIAN_POINT('Ctrl Pts',(2.33570088624363,2.22060436033124,301.71850172955));
#4216=CARTESIAN_POINT('Ctrl Pts',(2.32079313343711,2.2361801464205,301.719827752613));
#4217=CARTESIAN_POINT('Ctrl Pts',(2.27997095098759,2.27798361178716,301.723392142715));
#4218=CARTESIAN_POINT('Ctrl Pts',(2.25376021386129,2.30391884101336,301.725609529387));
#4219=CARTESIAN_POINT('Ctrl Pts',(2.09167769295594,2.45888384330308,301.738939017457));
#4220=CARTESIAN_POINT('Ctrl Pts',(1.94519681351087,2.57632489684497,301.749403057776));
#4221=CARTESIAN_POINT('Ctrl Pts',(1.62430013811067,2.79054410764109,301.771058122628));
#4222=CARTESIAN_POINT('Ctrl Pts',(1.44947065991038,2.8852230324201,301.782222005566));
#4223=CARTESIAN_POINT('Ctrl Pts',(1.21896518470082,2.98378566006795,301.797032378625));
#4224=CARTESIAN_POINT('Ctrl Pts',(1.17038442105278,3.00317379486243,301.800156288271));
#4225=CARTESIAN_POINT('Ctrl Pts',(1.0874739329138,3.03394529973871,301.805504018538));
#4226=CARTESIAN_POINT('Ctrl Pts',(1.05338452070672,3.04594887133107,301.807707301554));
#4227=CARTESIAN_POINT('Ctrl Pts',(0.987945107899092,3.06776149632866,301.811948647647));
#4228=CARTESIAN_POINT('Ctrl Pts',(0.956632753284695,3.0776695380587,301.813983191352));
#4229=CARTESIAN_POINT('Ctrl Pts',(0.873204846717059,3.10267213418293,301.819419792711));
#4230=CARTESIAN_POINT('Ctrl Pts',(0.820851999292563,3.11693158649496,301.822847722402));
#4231=CARTESIAN_POINT('Ctrl Pts',(0.534896372227233,3.18711408463789,301.841669465062));
#4232=CARTESIAN_POINT('Ctrl Pts',(0.295989141550298,3.21809975154081,301.857827407001));
#4233=CARTESIAN_POINT('Ctrl Pts',(-0.0458887649501769,3.22403113455179,
301.88087526916));
#4234=CARTESIAN_POINT('Ctrl Pts',(-0.147713212640572,3.22097271185103,301.887717702485));
#4235=CARTESIAN_POINT('Ctrl Pts',(-0.29270660207025,3.20972621046373,301.897305546022));
#4236=CARTESIAN_POINT('Ctrl Pts',(-0.336116277435697,3.20547121158965,301.900155702934));
#4237=CARTESIAN_POINT('Ctrl Pts',(-0.413891417913324,3.19625028357872,301.905211045777));
#4238=CARTESIAN_POINT('Ctrl Pts',(-0.448288151853629,3.19160773519085,301.907428721981));
#4239=CARTESIAN_POINT('Ctrl Pts',(-0.503480920506684,3.18324839413136,301.910951052349));
#4240=CARTESIAN_POINT('Ctrl Pts',(-0.524326378966687,3.17988133347345,301.9122730406));
#4241=CARTESIAN_POINT('Ctrl Pts',(-0.566392654434734,3.17266165670944,301.914921911329));
#4242=CARTESIAN_POINT('Ctrl Pts',(-0.587610786301522,3.16880044356729,301.916248298498));
#4243=CARTESIAN_POINT('Ctrl Pts',(-0.645024363515573,3.15775596017347,301.919814873786));
#4244=CARTESIAN_POINT('Ctrl Pts',(-0.68113880854343,3.15016337865994,301.922034037524));
#4245=CARTESIAN_POINT('Ctrl Pts',(-0.899161140598576,3.10040213866061,301.935326554268));
#4246=CARTESIAN_POINT('Ctrl Pts',(-1.07727074207155,3.04310484274677,301.94575668842));
#4247=CARTESIAN_POINT('Ctrl Pts',(-1.37294364717353,2.91874929396772,301.963759474257));
#4248=CARTESIAN_POINT('Ctrl Pts',(-1.49309270256789,2.85915080832196,301.971286435153));
#4249=CARTESIAN_POINT('Ctrl Pts',(-1.66348919025692,2.76095102586271,301.98261563099));
#4250=CARTESIAN_POINT('Ctrl Pts',(-1.71687264610595,2.72807524303073,301.986264769632));
#4251=CARTESIAN_POINT('Ctrl Pts',(-1.81382218260612,2.66439654580075,301.993110807778));
#4252=CARTESIAN_POINT('Ctrl Pts',(-1.85764772834944,2.63402815181,301.996292638502));
#4253=CARTESIAN_POINT('Ctrl Pts',(-1.93002503518077,2.58117022136455,302.001709139965));
#4254=CARTESIAN_POINT('Ctrl Pts',(-1.95898685052975,2.55925901464714,302.003921956551));
#4255=CARTESIAN_POINT('Ctrl Pts',(-2.01670583488942,2.51403758709401,302.008428313554));
#4256=CARTESIAN_POINT('Ctrl Pts',(-2.04544393430232,2.49071201613595,302.010722245879));
#4257=CARTESIAN_POINT('Ctrl Pts',(-2.11751906205271,2.43012276927658,302.01660820448));
#4258=CARTESIAN_POINT('Ctrl Pts',(-2.16027679763536,2.39219296059984,302.020226390257));
#4259=CARTESIAN_POINT('Ctrl Pts',(-2.35814107897976,2.20703784112354,302.037591905868));
#4260=CARTESIAN_POINT('Ctrl Pts',(-2.49932970715633,2.04576922141202,302.051915804817));
#4261=CARTESIAN_POINT('Ctrl Pts',(-2.72046649699764,1.73581633850882,302.077593112331));
#4262=CARTESIAN_POINT('Ctrl Pts',(-2.80673861025839,1.59255253214516,302.088856554702));
#4263=CARTESIAN_POINT('Ctrl Pts',(-2.89677624054073,1.41278622824015,302.101824726863));
#4264=CARTESIAN_POINT('Ctrl Pts',(-2.91154542266173,1.38209296957009,302.103999723996));
#4265=CARTESIAN_POINT('Ctrl Pts',(-2.9346238901664,1.33211881524392,302.107471533848));
#4266=CARTESIAN_POINT('Ctrl Pts',(-2.94323596838296,1.31298134997625,302.108784846463));
#4267=CARTESIAN_POINT('Ctrl Pts',(-2.96038181534689,1.27386380531314,302.111434481281));
#4268=CARTESIAN_POINT('Ctrl Pts',(-2.96890164483975,1.25387901008216,302.11277002841));
#4269=CARTESIAN_POINT('Ctrl Pts',(-2.99164140203908,1.199007275036,302.116391653468));
#4270=CARTESIAN_POINT('Ctrl Pts',(-3.0054531616125,1.16395373070989,302.118655586132));
#4271=CARTESIAN_POINT('Ctrl Pts',(-3.09930031094924,0.912956643547117,302.134569412469));
#4272=CARTESIAN_POINT('Ctrl Pts',(-3.15660877708911,0.689200884248465,302.147244531102));
#4273=CARTESIAN_POINT('Ctrl Pts',(-3.21161788323767,0.30878948818202,302.168896293925));
#4274=CARTESIAN_POINT('Ctrl Pts',(-3.22270289320938,0.154983159663994,302.17767059053));
#4275=CARTESIAN_POINT('Ctrl Pts',(-3.22276580278082,-0.0513356018517207,
302.189859200967));
#4276=CARTESIAN_POINT('Ctrl Pts',(-3.22150775251864,-0.10364416094275,302.192984082902));
#4277=CARTESIAN_POINT('Ctrl Pts',(-3.21722876997443,-0.191997104707538,
302.198332964639));
#4278=CARTESIAN_POINT('Ctrl Pts',(-3.21487331077823,-0.228064203310865,
302.200536404917));
#4279=CARTESIAN_POINT('Ctrl Pts',(-3.20922094147811,-0.296811200111426,
302.204777712067));
#4280=CARTESIAN_POINT('Ctrl Pts',(-3.20603003806182,-0.329495387503727,
302.206812053817));
#4281=CARTESIAN_POINT('Ctrl Pts',(-3.19624613172568,-0.416016527269546,
302.212247272874));
#4282=CARTESIAN_POINT('Ctrl Pts',(-3.1887927799652,-0.469743691384225,302.215673997404));
#4283=CARTESIAN_POINT('Ctrl Pts',(-3.14096708145004,-0.760395850071991,
302.234503004226));
#4284=CARTESIAN_POINT('Ctrl Pts',(-3.07554765739168,-0.992395016090034,
302.250670481751));
#4285=CARTESIAN_POINT('Ctrl Pts',(-2.94661817863001,-1.30916417782987,302.273723134994));
#4286=CARTESIAN_POINT('Ctrl Pts',(-2.90381901916496,-1.40153719398589,302.280561153221));
#4287=CARTESIAN_POINT('Ctrl Pts',(-2.83654024802534,-1.53037824036094,302.290143628212));
#4288=CARTESIAN_POINT('Ctrl Pts',(-2.81557790831675,-1.56861069688823,302.292992726357));
#4289=CARTESIAN_POINT('Ctrl Pts',(-2.77655110855963,-1.63648564947723,302.298046411385));
#4290=CARTESIAN_POINT('Ctrl Pts',(-2.75877143845277,-1.66628380263649,302.300263477205));
#4291=CARTESIAN_POINT('Ctrl Pts',(-2.72940399550728,-1.71374359994853,302.303785084261));
#4292=CARTESIAN_POINT('Ctrl Pts',(-2.71811818269049,-1.73158797427979,302.305106947595));
#4293=CARTESIAN_POINT('Ctrl Pts',(-2.69495043300568,-1.76743454884903,302.307755823025));
#4294=CARTESIAN_POINT('Ctrl Pts',(-2.68306157868412,-1.78543085730189,302.309082335909));
#4295=CARTESIAN_POINT('Ctrl Pts',(-2.65033935025029,-1.83389782787387,302.312649665728));
#4296=CARTESIAN_POINT('Ctrl Pts',(-2.62916114697263,-1.86413299773039,302.314869443073));
#4297=CARTESIAN_POINT('Ctrl Pts',(-2.4978730182205,-2.04487727651015,302.328147853828));
#4298=CARTESIAN_POINT('Ctrl Pts',(-2.375377668476,-2.18597546425527,302.338565095895));
#4299=CARTESIAN_POINT('Ctrl Pts',(-2.09779979157631,-2.45464190113278,302.360246544473));
#4300=CARTESIAN_POINT('Ctrl Pts',(-1.94165263881097,-2.57992354549356,302.371484735465));
#4301=CARTESIAN_POINT('Ctrl Pts',(-1.73147175570793,-2.71860863098421,302.386364689123));
#4302=CARTESIAN_POINT('Ctrl Pts',(-1.68733624352936,-2.74621981728922,302.38947452305));
#4303=CARTESIAN_POINT('Ctrl Pts',(-1.61149581100998,-2.79114705121563,302.394805595799));
#4304=CARTESIAN_POINT('Ctrl Pts',(-1.58013257040606,-2.80902145052584,302.39700661366));
#4305=CARTESIAN_POINT('Ctrl Pts',(-1.5243051829562,-2.83960752620019,302.400921189997));
#4306=CARTESIAN_POINT('Ctrl Pts',(-1.49996563704107,-2.85253925179863,302.402626772245));
#4307=CARTESIAN_POINT('Ctrl Pts',(-1.47546400229876,-2.86515680904563,302.404343180173));
#4308=CARTESIAN_POINT('Origin',(0.,0.,294.689226550727));
#4309=CARTESIAN_POINT('',(-1.47546400670695,-2.86515680677555,303.903774856397));
#4310=CARTESIAN_POINT('',(-1.47546383039573,-2.86515689757018,303.659226720281));
#4311=CARTESIAN_POINT('',(-1.47546400239267,-2.86515680899727,294.689226550727));
#4312=CARTESIAN_POINT('',(3.22274978263189,0.00118365792144974,303.057982460212));
#4313=CARTESIAN_POINT('Ctrl Pts',(-1.47546400670695,-2.86515680677555,303.903774856397));
#4314=CARTESIAN_POINT('Ctrl Pts',(-1.64703992383269,-2.7768007037036,303.890776726147));
#4315=CARTESIAN_POINT('Ctrl Pts',(-1.81035156217509,-2.67320167904195,303.877671639076));
#4316=CARTESIAN_POINT('Ctrl Pts',(-1.99185243055068,-2.53375739307966,303.862879504612));
#4317=CARTESIAN_POINT('Ctrl Pts',(-2.01991429026229,-2.51144363538858,303.860586313955));
#4318=CARTESIAN_POINT('Ctrl Pts',(-2.06407442531159,-2.47510999874109,303.856975206977));
#4319=CARTESIAN_POINT('Ctrl Pts',(-2.08041512192467,-2.46139101297975,303.855638448391));
#4320=CARTESIAN_POINT('Ctrl Pts',(-2.11278122990651,-2.43366512642933,303.852991729229));
#4321=CARTESIAN_POINT('Ctrl Pts',(-2.12880653300698,-2.419659743581,303.851681786262));
#4322=CARTESIAN_POINT('Ctrl Pts',(-2.17125751362461,-2.38181129630646,303.848209470128));
#4323=CARTESIAN_POINT('Ctrl Pts',(-2.19742966188655,-2.35768686517194,303.846066283176));
#4324=CARTESIAN_POINT('Ctrl Pts',(-2.25586995852725,-2.30200021413352,303.841260646555));
#4325=CARTESIAN_POINT('Ctrl Pts',(-2.28788587475091,-2.2701834376632,303.838613456726));
#4326=CARTESIAN_POINT('Ctrl Pts',(-2.394351410733,-2.15983929400474,303.829716810863));
#4327=CARTESIAN_POINT('Ctrl Pts',(-2.46551386365164,-2.07823684474175,303.82360670651));
#4328=CARTESIAN_POINT('Ctrl Pts',(-2.67292206994574,-1.81471718757523,303.804756006067));
#4329=CARTESIAN_POINT('Ctrl Pts',(-2.79412955370635,-1.62189440690968,303.792115830217));
#4330=CARTESIAN_POINT('Ctrl Pts',(-2.91863148260553,-1.36778190217344,303.775452500689));
#4331=CARTESIAN_POINT('Ctrl Pts',(-2.94189616456491,-1.31699790374123,303.772125479833));
#4332=CARTESIAN_POINT('Ctrl Pts',(-2.97825921934005,-1.23184406484862,303.766536927087));
#4333=CARTESIAN_POINT('Ctrl Pts',(-2.99211032432934,-1.19780775416496,303.764300677367));
#4334=CARTESIAN_POINT('Ctrl Pts',(-3.01854345939051,-1.12953223310251,303.759806225724));
#4335=CARTESIAN_POINT('Ctrl Pts',(-3.031132167772,-1.09530146220508,303.757548643026));
#4336=CARTESIAN_POINT('Ctrl Pts',(-3.06102519918106,-1.00955205574303,303.751879697221));
#4337=CARTESIAN_POINT('Ctrl Pts',(-3.07761189331703,-0.957797002403391,
303.748445944007));
#4338=CARTESIAN_POINT('Ctrl Pts',(-3.1109669885766,-0.843886120364744,303.740857926401));
#4339=CARTESIAN_POINT('Ctrl Pts',(-3.12719730379387,-0.781598080957308,
303.736689150671));
#4340=CARTESIAN_POINT('Ctrl Pts',(-3.17299354537236,-0.58146253220149,303.723239028106));
#4341=CARTESIAN_POINT('Ctrl Pts',(-3.19538468486823,-0.442151313892892,
303.713785752114));
#4342=CARTESIAN_POINT('Ctrl Pts',(-3.22480127742499,-0.129443062851917,
303.692611258972));
#4343=CARTESIAN_POINT('Ctrl Pts',(-3.22709965554132,0.0439846905240419,
303.680894853082));
#4344=CARTESIAN_POINT('Ctrl Pts',(-3.21286988157641,0.255064913389759,303.66718715784));
#4345=CARTESIAN_POINT('Ctrl Pts',(-3.20960387595817,0.293315932480469,303.664726205883));
#4346=CARTESIAN_POINT('Ctrl Pts',(-3.20340692144339,0.353241186111654,303.660916246447));
#4347=CARTESIAN_POINT('Ctrl Pts',(-3.20093759968591,0.374958378955537,303.659544907881));
#4348=CARTESIAN_POINT('Ctrl Pts',(-3.19568167654034,0.417337718593409,303.656889435075));
#4349=CARTESIAN_POINT('Ctrl Pts',(-3.19291518748996,0.438000896554211,303.655604436301));
#4350=CARTESIAN_POINT('Ctrl Pts',(-3.18519130253673,0.491722767386906,303.652285738227));
#4351=CARTESIAN_POINT('Ctrl Pts',(-3.17991957596055,0.524734789674906,303.650268269316));
#4352=CARTESIAN_POINT('Ctrl Pts',(-3.16695752725866,0.59851321161376,303.64579666514));
#4353=CARTESIAN_POINT('Ctrl Pts',(-3.15899176796981,0.639225583198342,303.643354778871));
#4354=CARTESIAN_POINT('Ctrl Pts',(-3.13054138666105,0.771071636469618,303.635497985669));
#4355=CARTESIAN_POINT('Ctrl Pts',(-3.10688019852166,0.86147442372401,303.630190172295));
#4356=CARTESIAN_POINT('Ctrl Pts',(-3.00286087530714,1.198384530277,303.610306744584));
#4357=CARTESIAN_POINT('Ctrl Pts',(-2.89680882073736,1.43589304542686,303.595991172968));
#4358=CARTESIAN_POINT('Ctrl Pts',(-2.73695103401422,1.70231349000082,303.577622383332));
#4359=CARTESIAN_POINT('Ctrl Pts',(-2.70938750585779,1.7458496759023,303.574543090492));
#4360=CARTESIAN_POINT('Ctrl Pts',(-2.66102150797335,1.81833745998218,303.569271389652));
#4361=CARTESIAN_POINT('Ctrl Pts',(-2.64076035919025,1.84763934655529,303.567098898376));
#4362=CARTESIAN_POINT('Ctrl Pts',(-2.59829348237041,1.90692959583001,303.56261376611));
#4363=CARTESIAN_POINT('Ctrl Pts',(-2.57604440063986,1.93688011177592,303.560299704713));
#4364=CARTESIAN_POINT('Ctrl Pts',(-2.51735578698527,2.01308318969035,303.554282414172));
#4365=CARTESIAN_POINT('Ctrl Pts',(-2.48016092469924,2.05873387465501,303.550550570188));
#4366=CARTESIAN_POINT('Ctrl Pts',(-2.39485184176819,2.15776810772177,303.542162267115));
#4367=CARTESIAN_POINT('Ctrl Pts',(-2.3461611812047,2.21061193287783,303.537485353967));
#4368=CARTESIAN_POINT('Ctrl Pts',(-2.17165758768544,2.3877361262764,303.521107428813));
#4369=CARTESIAN_POINT('Ctrl Pts',(-2.03741862728109,2.50325740162402,303.509137394115));
#4370=CARTESIAN_POINT('Ctrl Pts',(-1.78757615510471,2.68479498467136,303.488350790574));
#4371=CARTESIAN_POINT('Ctrl Pts',(-1.6760762210895,2.75578070158462,303.479528749445));
#4372=CARTESIAN_POINT('Ctrl Pts',(-1.53227791175949,2.83536317818561,303.468949705946));
#4373=CARTESIAN_POINT('Ctrl Pts',(-1.50379480462413,2.85057210371432,303.466891539695));
#4374=CARTESIAN_POINT('Ctrl Pts',(-1.45855309369064,2.87386259992281,303.463686244889));
#4375=CARTESIAN_POINT('Ctrl Pts',(-1.44194552686641,2.88223116956595,303.462522962458));
#4376=CARTESIAN_POINT('Ctrl Pts',(-1.40600598591886,2.89995273510034,303.46003565169));
#4377=CARTESIAN_POINT('Ctrl Pts',(-1.38665101833263,2.90925724392156,303.45871461091));
#4378=CARTESIAN_POINT('Ctrl Pts',(-1.33413101749682,2.93386193774287,303.455175808777));
#4379=CARTESIAN_POINT('Ctrl Pts',(-1.30079562116827,2.94879338742762,303.45297854448));
#4380=CARTESIAN_POINT('Ctrl Pts',(-1.22424109596349,2.98153241039079,303.448027349343));
#4381=CARTESIAN_POINT('Ctrl Pts',(-1.18087347722927,2.99897315751643,303.445290097142));
#4382=CARTESIAN_POINT('Ctrl Pts',(-1.02931135345218,3.05612763916361,303.435906749962));
#4383=CARTESIAN_POINT('Ctrl Pts',(-0.919373295761669,3.09097939198203,303.42941634474));
#4384=CARTESIAN_POINT('Ctrl Pts',(-0.600456048695917,3.17355376570913,303.410914511226));
#4385=CARTESIAN_POINT('Ctrl Pts',(-0.388296340070686,3.20643223628765,303.39895783596));
#4386=CARTESIAN_POINT('Ctrl Pts',(-0.117435068217946,3.2211157927311,303.383001384459));
#4387=CARTESIAN_POINT('Ctrl Pts',(-0.0603496933341818,3.2226906901211,303.379603082123));
#4388=CARTESIAN_POINT('Ctrl Pts',(0.0337208880234273,3.22278570215275,303.373928736213));
#4389=CARTESIAN_POINT('Ctrl Pts',(0.0706934557232164,3.22218668669088,303.371679700065));
#4390=CARTESIAN_POINT('Ctrl Pts',(0.143900989283213,3.21974004080657,303.367185367169));
#4391=CARTESIAN_POINT('Ctrl Pts',(0.180131311604691,3.21791640168691,303.364941134504));
#4392=CARTESIAN_POINT('Ctrl Pts',(0.269440640683299,3.21190810299397,303.359356537013));
#4393=CARTESIAN_POINT('Ctrl Pts',(0.322459902247589,3.2070190217009,303.355995225971));
#4394=CARTESIAN_POINT('Ctrl Pts',(0.437488160306886,3.19353068860341,303.348598520563));
#4395=CARTESIAN_POINT('Ctrl Pts',(0.499416054034859,3.18443353923819,303.344549887132));
#4396=CARTESIAN_POINT('Ctrl Pts',(0.69264604506215,3.15027321482627,303.331712896561));
#4397=CARTESIAN_POINT('Ctrl Pts',(0.822670594343443,3.11884399761831,303.322769933577));
#4398=CARTESIAN_POINT('Ctrl Pts',(1.12941154473084,3.02417928932736,303.301142764094));
#4399=CARTESIAN_POINT('Ctrl Pts',(1.30331426887408,2.95340679198056,303.28843040933));
#4400=CARTESIAN_POINT('Ctrl Pts',(1.50288317194297,2.85110816200811,303.273921908207));
#4401=CARTESIAN_POINT('Ctrl Pts',(1.53538791899156,2.83373601075532,303.271562408484));
#4402=CARTESIAN_POINT('Ctrl Pts',(1.58641073614623,2.80533110137519,303.267872594399));
#4403=CARTESIAN_POINT('Ctrl Pts',(1.60512752506377,2.79466407661601,303.26652208425));
#4404=CARTESIAN_POINT('Ctrl Pts',(1.64195544782887,2.77318313942054,303.263872912534));
#4405=CARTESIAN_POINT('Ctrl Pts',(1.6600700306086,2.76237759095298,303.262573908045));
#4406=CARTESIAN_POINT('Ctrl Pts',(1.70766798804779,2.73334756135107,303.259167879495));
#4407=CARTESIAN_POINT('Ctrl Pts',(1.73696657071128,2.71482341897815,303.257078753184));
#4408=CARTESIAN_POINT('Ctrl Pts',(1.80238803500374,2.67196766076223,303.252417487722));
#4409=CARTESIAN_POINT('Ctrl Pts',(1.83832841668652,2.64736902820155,303.249859265508));
#4410=CARTESIAN_POINT('Ctrl Pts',(1.95641024736844,2.56298573211447,303.241424360068));
#4411=CARTESIAN_POINT('Ctrl Pts',(2.03622569171254,2.50004482069593,303.235672250693));
#4412=CARTESIAN_POINT('Ctrl Pts',(2.29468205859889,2.27562862774268,303.216408777792));
#4413=CARTESIAN_POINT('Ctrl Pts',(2.45815980934174,2.09797339487428,303.20305713722));
#4414=CARTESIAN_POINT('Ctrl Pts',(2.63232887658665,1.86007948301842,303.185669195881));
#4415=CARTESIAN_POINT('Ctrl Pts',(2.66321540827956,1.81558095090272,303.182438896499));
#4416=CARTESIAN_POINT('Ctrl Pts',(2.71098388656152,1.74291707379026,303.177185895728));
#4417=CARTESIAN_POINT('Ctrl Pts',(2.72858289538505,1.71523433448492,303.175189635818));
#4418=CARTESIAN_POINT('Ctrl Pts',(2.76465978944355,1.65652573818348,303.170963599017));
#4419=CARTESIAN_POINT('Ctrl Pts',(2.78304481718737,1.62544844677601,303.168730866642));
#4420=CARTESIAN_POINT('Ctrl Pts',(2.82675793581253,1.54864113352191,303.163220054273));
#4421=CARTESIAN_POINT('Ctrl Pts',(2.85150228505659,1.50259242887546,303.159922273455));
#4422=CARTESIAN_POINT('Ctrl Pts',(2.90269117303861,1.40150895993529,303.152692392094));
#4423=CARTESIAN_POINT('Ctrl Pts',(2.9287133903155,1.34628397887262,303.148748116728));
#4424=CARTESIAN_POINT('Ctrl Pts',(3.00423160533578,1.17345054718622,303.136424941579));
#4425=CARTESIAN_POINT('Ctrl Pts',(3.04832181703954,1.05362384471593,303.127905208829));
#4426=CARTESIAN_POINT('Ctrl Pts',(3.10129921026084,0.87816069803812,303.115567252037));
#4427=CARTESIAN_POINT('Ctrl Pts',(3.11602001096471,0.824404178271397,303.111806264146));
#4428=CARTESIAN_POINT('Ctrl Pts',(3.12974010974781,0.768665868225409,303.107937075732));
#4429=CARTESIAN_POINT('Ctrl Pts',(3.13013943786739,0.767038115772963,303.107824108745));
#4430=CARTESIAN_POINT('Ctrl Pts',(3.14965191724887,0.687231810421434,303.102286831792));
#4431=CARTESIAN_POINT('Ctrl Pts',(3.16583175498072,0.608362453887039,303.096876159802));
#4432=CARTESIAN_POINT('Ctrl Pts',(3.19152114932299,0.453971854317972,303.086484531808));
#4433=CARTESIAN_POINT('Ctrl Pts',(3.20134314521489,0.37855183052115,303.081499602661));
#4434=CARTESIAN_POINT('Ctrl Pts',(3.2111672238192,0.274472358776477,303.074803934069));
#4435=CARTESIAN_POINT('Ctrl Pts',(3.21346928796665,0.246059504636998,303.072994818867));
#4436=CARTESIAN_POINT('Ctrl Pts',(3.21672359690848,0.197975935185697,303.069968997583));
#4437=CARTESIAN_POINT('Ctrl Pts',(3.21787304032332,0.178320897428194,303.068742345663));
#4438=CARTESIAN_POINT('Ctrl Pts',(3.21976697660709,0.139896146143514,303.066365017933));
#4439=CARTESIAN_POINT('Ctrl Pts',(3.22052761665186,0.12112895931221,303.065213288147));
#4440=CARTESIAN_POINT('Ctrl Pts',(3.22219541480293,0.068643499314685,303.062015894739));
#4441=CARTESIAN_POINT('Ctrl Pts',(3.22273739359673,0.0349153296029804,303.059988401622));
#4442=CARTESIAN_POINT('Ctrl Pts',(3.22274978263189,0.00118365792144974,
303.057982460212));
#4443=CARTESIAN_POINT('Ctrl Pts',(3.22274978135357,0.0011871333156251,303.057982666885));
#4444=CARTESIAN_POINT('Ctrl Pts',(3.22282215967534,-0.195300672711181,303.046298000788));
#4445=CARTESIAN_POINT('Ctrl Pts',(3.20492489689649,-0.39141482917079,303.035355889149));
#4446=CARTESIAN_POINT('Ctrl Pts',(3.14597524532254,-0.710940044934372,303.017115073304));
#4447=CARTESIAN_POINT('Ctrl Pts',(3.11516470245604,-0.835668823371542,303.009889828884));
#4448=CARTESIAN_POINT('Ctrl Pts',(3.05878981325368,-1.01669727728896,302.998954718108));
#4449=CARTESIAN_POINT('Ctrl Pts',(3.03891752920731,-1.07463860111911,302.995385414962));
#4450=CARTESIAN_POINT('Ctrl Pts',(2.99900211799949,-1.18103751210788,302.988672598943));
#4451=CARTESIAN_POINT('Ctrl Pts',(2.97940391253876,-1.22964026481056,302.985543098519));
#4452=CARTESIAN_POINT('Ctrl Pts',(2.94430605617543,-1.31090988304529,302.9801904342));
#4453=CARTESIAN_POINT('Ctrl Pts',(2.92942547827781,-1.34383372481131,302.977987961534));
#4454=CARTESIAN_POINT('Ctrl Pts',(2.89999399256367,-1.40613901762976,302.973751381266));
#4455=CARTESIAN_POINT('Ctrl Pts',(2.88554201781415,-1.43556234051875,302.971720838681));
#4456=CARTESIAN_POINT('Ctrl Pts',(2.84609044767663,-1.51287976787604,302.966303088094));
#4457=CARTESIAN_POINT('Ctrl Pts',(2.82033191745928,-1.56037282525552,302.962890297893));
#4458=CARTESIAN_POINT('Ctrl Pts',(2.67283357490284,-1.81673320848036,302.943987694369));
#4459=CARTESIAN_POINT('Ctrl Pts',(2.52909632679752,-2.01201272774872,302.927721540704));
#4460=CARTESIAN_POINT('Ctrl Pts',(2.29623140226047,-2.26355059429498,302.904617794217));
#4461=CARTESIAN_POINT('Ctrl Pts',(2.22408910706801,-2.33447412570847,302.897823960675));
#4462=CARTESIAN_POINT('Ctrl Pts',(2.11636223527207,-2.43084644778694,302.88829597584));
#4463=CARTESIAN_POINT('Ctrl Pts',(2.08341213465356,-2.45914574121506,302.885458206472));
#4464=CARTESIAN_POINT('Ctrl Pts',(2.02320811965574,-2.50877319129619,302.880422682717));
#4465=CARTESIAN_POINT('Ctrl Pts',(1.99616380274306,-2.53034470235584,302.878212562607));
#4466=CARTESIAN_POINT('Ctrl Pts',(1.95208924029284,-2.56435360433839,302.874700045792));
#4467=CARTESIAN_POINT('Ctrl Pts',(1.93527568376051,-2.57706614370546,302.873380452149));
#4468=CARTESIAN_POINT('Ctrl Pts',(1.90101496141205,-2.6024458570146,302.870734430252));
#4469=CARTESIAN_POINT('Ctrl Pts',(1.88356309473785,-2.61510467298162,302.869408525631));
#4470=CARTESIAN_POINT('Ctrl Pts',(1.83587386969106,-2.64897123900244,302.865840548283));
#4471=CARTESIAN_POINT('Ctrl Pts',(1.80539602270693,-2.66983650200855,302.863619557783));
#4472=CARTESIAN_POINT('Ctrl Pts',(1.61973046894774,-2.79231019303226,302.8503994142));
#4473=CARTESIAN_POINT('Ctrl Pts',(1.45635000823409,-2.88089961067451,302.840034391468));
#4474=CARTESIAN_POINT('Ctrl Pts',(1.16269295093685,-3.00872373829066,302.822059298298));
#4475=CARTESIAN_POINT('Ctrl Pts',(1.03589936654935,-3.05469857648612,302.814492063085));
#4476=CARTESIAN_POINT('Ctrl Pts',(0.846290048557142,-3.11028317168793,302.803111409237));
#4477=CARTESIAN_POINT('Ctrl Pts',(0.785472195981641,-3.12619593767203,302.799452838664));
#4478=CARTESIAN_POINT('Ctrl Pts',(0.672187800579716,-3.15232193788623,302.792591819323));
#4479=CARTESIAN_POINT('Ctrl Pts',(0.619857332590626,-3.16302805046279,302.789404582625));
#4480=CARTESIAN_POINT('Ctrl Pts',(0.53154926625777,-3.17881911603224,302.783983312327));
#4481=CARTESIAN_POINT('Ctrl Pts',(0.495707161687191,-3.1846051311663,302.781771284133));
#4482=CARTESIAN_POINT('Ctrl Pts',(0.423215331552128,-3.1950541156918,302.777270376426));
#4483=CARTESIAN_POINT('Ctrl Pts',(0.386567977348554,-3.19969483559144,302.774981169959));
#4484=CARTESIAN_POINT('Ctrl Pts',(0.293287485980368,-3.20988122754678,302.769116063972));
#4485=CARTESIAN_POINT('Ctrl Pts',(0.236574230213031,-3.21455860695353,302.765514324017));
#4486=CARTESIAN_POINT('Ctrl Pts',(-0.036566787012202,-3.22981856003294,
302.747986798995));
#4487=CARTESIAN_POINT('Ctrl Pts',(-0.253541444060071,-3.22005530422065,
302.733465946025));
#4488=CARTESIAN_POINT('Ctrl Pts',(-0.630607992416144,-3.1647287216089,302.707764851886));
#4489=CARTESIAN_POINT('Ctrl Pts',(-0.791301066712531,-3.12842222518099,
302.696674878214));
#4490=CARTESIAN_POINT('Ctrl Pts',(-0.981135095872506,-3.06996016606138,
302.683861922834));
#4491=CARTESIAN_POINT('Ctrl Pts',(-1.0135804364278,-3.05940131524089,302.681683042893));
#4492=CARTESIAN_POINT('Ctrl Pts',(-1.06569997050893,-3.04151958504009,302.678207510384));
#4493=CARTESIAN_POINT('Ctrl Pts',(-1.08548039255301,-3.03451646987384,302.67689427096));
#4494=CARTESIAN_POINT('Ctrl Pts',(-1.12555158747701,-3.01988757260093,302.674247707146));
#4495=CARTESIAN_POINT('Ctrl Pts',(-1.14583647819923,-3.01224935116519,302.672915110734));
#4496=CARTESIAN_POINT('Ctrl Pts',(-1.20099843193554,-2.9908403885497,302.669306930165));
#4497=CARTESIAN_POINT('Ctrl Pts',(-1.23571569256085,-2.97666431713816,302.667053245252));
#4498=CARTESIAN_POINT('Ctrl Pts',(-1.33974785891755,-2.93205100418127,302.66032965188));
#4499=CARTESIAN_POINT('Ctrl Pts',(-1.40821778573291,-2.8997864605469,302.65594455659));
#4500=CARTESIAN_POINT('Ctrl Pts',(-1.47546411936631,-2.86515674875958,302.651619072379));
#4501=CARTESIAN_POINT('Ctrl Pts',(-1.47546400229876,-2.86515680904563,302.404343180173));
#4502=CARTESIAN_POINT('Ctrl Pts',(-1.47073118624233,-2.86759405775003,302.404674727153));
#4503=CARTESIAN_POINT('Ctrl Pts',(-1.46599232228165,-2.87001958418981,302.405006677517));
#4504=CARTESIAN_POINT('Ctrl Pts',(-1.41265079463178,-2.89715517325867,302.408742979947));
#4505=CARTESIAN_POINT('Ctrl Pts',(-1.36343707625227,-2.92063848148305,302.412188592157));
#4506=CARTESIAN_POINT('Ctrl Pts',(-1.09617202871527,-3.03994200400015,302.43090242102));
#4507=CARTESIAN_POINT('Ctrl Pts',(-0.86862901796382,-3.11260185013267,302.446919076186));
#4508=CARTESIAN_POINT('Ctrl Pts',(-0.534459251722771,-3.17978471014962,
302.469896306618));
#4509=CARTESIAN_POINT('Ctrl Pts',(-0.432797805361918,-3.19520976496153,
302.476804626933));
#4510=CARTESIAN_POINT('Ctrl Pts',(-0.286956688052462,-3.21024854093123,
302.486472526695));
#4511=CARTESIAN_POINT('Ctrl Pts',(-0.243254973779329,-3.2138555034111,302.489338426503));
#4512=CARTESIAN_POINT('Ctrl Pts',(-0.164716151259587,-3.21872647520065,
302.494418409729));
#4513=CARTESIAN_POINT('Ctrl Pts',(-0.129906570391553,-3.22031924493887,
302.496645152468));
#4514=CARTESIAN_POINT('Ctrl Pts',(-0.0739435201431905,-3.22197096638263,
302.500178229253));
#4515=CARTESIAN_POINT('Ctrl Pts',(-0.0528041435150932,-3.22238674650866,
302.501502075628));
#4516=CARTESIAN_POINT('Ctrl Pts',(-0.0101291085400843,-3.22280602078181,
302.50415089681));
#4517=CARTESIAN_POINT('Ctrl Pts',(0.0114054518002629,-3.22280176589306,
302.505475433915));
#4518=CARTESIAN_POINT('Ctrl Pts',(0.0696809240949528,-3.22220611352631,
302.509030908092));
#4519=CARTESIAN_POINT('Ctrl Pts',(0.10641542374083,-3.22120221022146,302.511241044003));
#4520=CARTESIAN_POINT('Ctrl Pts',(0.332366381158546,-3.21115753204423,302.524687294124));
#4521=CARTESIAN_POINT('Ctrl Pts',(0.520517618063955,-3.18607552435117,302.535259539811));
#4522=CARTESIAN_POINT('Ctrl Pts',(0.834655131401481,-3.11560879406432,302.553329585848));
#4523=CARTESIAN_POINT('Ctrl Pts',(0.962002931064495,-3.07867100874392,302.560775190834));
#4524=CARTESIAN_POINT('Ctrl Pts',(1.14536707144118,-3.01299415473027,302.571998593587));
#4525=CARTESIAN_POINT('Ctrl Pts',(1.20339906949475,-2.99028920927167,302.575626733216));
#4526=CARTESIAN_POINT('Ctrl Pts',(1.30958088626837,-2.94515408251542,302.582437933963));
#4527=CARTESIAN_POINT('Ctrl Pts',(1.35790484512252,-2.92318809327359,302.585606211378));
#4528=CARTESIAN_POINT('Ctrl Pts',(1.4383038180321,-2.88421834563816,302.591006589947));
#4529=CARTESIAN_POINT('Ctrl Pts',(1.47067467203613,-2.86784748275387,302.593217147003));
#4530=CARTESIAN_POINT('Ctrl Pts',(1.53554975619119,-2.83365105415766,302.597724720318));
#4531=CARTESIAN_POINT('Ctrl Pts',(1.56803644807082,-2.81580412477582,302.600022227241));
#4532=CARTESIAN_POINT('Ctrl Pts',(1.65006177195242,-2.76888289886511,302.605930131731));
#4533=CARTESIAN_POINT('Ctrl Pts',(1.69914248232862,-2.73903824824186,302.609567085062));
#4534=CARTESIAN_POINT('Ctrl Pts',(1.9235588087959,-2.59422325144197,302.626686718665));
#4535=CARTESIAN_POINT('Ctrl Pts',(2.08818379566014,-2.46364320786856,302.640719492988));
#4536=CARTESIAN_POINT('Ctrl Pts',(2.32374576687523,-2.23611808026006,302.662804903421));
#4537=CARTESIAN_POINT('Ctrl Pts',(2.40399355096707,-2.14961288248822,302.670760825514));
#4538=CARTESIAN_POINT('Ctrl Pts',(2.50956150784151,-2.02248830197332,302.6816874032));
#4539=CARTESIAN_POINT('Ctrl Pts',(2.53899591464482,-1.98541130565433,302.684789793274));
#4540=CARTESIAN_POINT('Ctrl Pts',(2.58988827498364,-1.91832110299869,302.690237741653));
#4541=CARTESIAN_POINT('Ctrl Pts',(2.61166768733984,-1.88856275588037,302.692598608586));
#4542=CARTESIAN_POINT('Ctrl Pts',(2.64536526867472,-1.84082182232138,302.696290891586));
#4543=CARTESIAN_POINT('Ctrl Pts',(2.65762130397304,-1.8230829525313,302.69764252059));
#4544=CARTESIAN_POINT('Ctrl Pts',(2.68010611390223,-1.78983071272968,302.700136685735));
#4545=CARTESIAN_POINT('Ctrl Pts',(2.69038036243288,-1.77434954194624,302.701282176299));
#4546=CARTESIAN_POINT('Ctrl Pts',(2.71804315638984,-1.73187468052494,302.704384854147));
#4547=CARTESIAN_POINT('Ctrl Pts',(2.73516361706921,-1.70470779669856,302.706325639925));
#4548=CARTESIAN_POINT('Ctrl Pts',(2.81653828565511,-1.57119886370915,302.715675644608));
#4549=CARTESIAN_POINT('Ctrl Pts',(2.87501821711156,-1.46144792323411,302.722791891237));
#4550=CARTESIAN_POINT('Ctrl Pts',(2.98285306220959,-1.22739909297677,302.737362824025));
#4551=CARTESIAN_POINT('Ctrl Pts',(3.0311078479289,-1.10286296536373,302.744791730176));
#4552=CARTESIAN_POINT('Ctrl Pts',(3.11528559822034,-0.837869584490296,302.760498505911));
#4553=CARTESIAN_POINT('Ctrl Pts',(3.14973659919007,-0.697268268618499,302.768779802692));
#4554=CARTESIAN_POINT('Ctrl Pts',(3.18307834439978,-0.506495929627978,302.780257793227));
#4555=CARTESIAN_POINT('Ctrl Pts',(3.19042151169116,-0.457969510802434,302.783196887772));
#4556=CARTESIAN_POINT('Ctrl Pts',(3.20117748000664,-0.373964071771196,302.788328118672));
#4557=CARTESIAN_POINT('Ctrl Pts',(3.20511512978323,-0.338560533890505,302.790503780196));
#4558=CARTESIAN_POINT('Ctrl Pts',(3.21205961313571,-0.265049717864161,302.795051718627));
#4559=CARTESIAN_POINT('Ctrl Pts',(3.21497689582935,-0.226939802926653,302.797426387712));
#4560=CARTESIAN_POINT('Ctrl Pts',(3.22093863610593,-0.125343420396632,302.803805373462));
#4561=CARTESIAN_POINT('Ctrl Pts',(3.22278385710846,-0.0618061141021424,
302.807845217358));
#4562=CARTESIAN_POINT('Ctrl Pts',(3.22261075162948,0.25864997648741,302.828484081738));
#4563=CARTESIAN_POINT('Ctrl Pts',(3.19175126853861,0.514593732784742,302.845924818716));
#4564=CARTESIAN_POINT('Ctrl Pts',(3.10330441094823,0.876996154347947,302.870975938121));
#4565=CARTESIAN_POINT('Ctrl Pts',(3.0696650687625,0.988322617464399,302.878704430591));
#4566=CARTESIAN_POINT('Ctrl Pts',(3.01926688378704,1.12745442980147,302.888223283326));
#4567=CARTESIAN_POINT('Ctrl Pts',(3.00801029837313,1.15715177289447,302.890246489179));
#4568=CARTESIAN_POINT('Ctrl Pts',(2.98882481859061,1.20559432260662,302.893527139406));
#4569=CARTESIAN_POINT('Ctrl Pts',(2.98115425020853,1.22443900955153,302.894798374417));
#4570=CARTESIAN_POINT('Ctrl Pts',(2.96469060871092,1.26381401286018,302.897442417982));
#4571=CARTESIAN_POINT('Ctrl Pts',(2.95586173361889,1.28432773945447,302.898813185237));
#4572=CARTESIAN_POINT('Ctrl Pts',(2.9303515257064,1.34194342556025,302.902648568309));
#4573=CARTESIAN_POINT('Ctrl Pts',(2.91317944215478,1.37882489511807,302.90508646073));
#4574=CARTESIAN_POINT('Ctrl Pts',(2.8715341634513,1.46401522768814,302.910699278798));
#4575=CARTESIAN_POINT('Ctrl Pts',(2.84653229818124,1.51205273629969,302.913850255582));
#4576=CARTESIAN_POINT('Ctrl Pts',(2.74617891591497,1.69354724448225,302.925784793454));
#4577=CARTESIAN_POINT('Ctrl Pts',(2.66255291101688,1.82220122979056,302.934315251613));
#4578=CARTESIAN_POINT('Ctrl Pts',(2.47339160539816,2.07222983097413,302.951938808824));
#4579=CARTESIAN_POINT('Ctrl Pts',(2.36730662596435,2.19263660830288,302.961018786929));
#4580=CARTESIAN_POINT('Ctrl Pts',(2.21147956025781,2.34495208503251,302.973830815243));
#4581=CARTESIAN_POINT('Ctrl Pts',(2.16917432184813,2.38414015872624,302.97726110704));
#4582=CARTESIAN_POINT('Ctrl Pts',(2.09795386841559,2.44664750544897,302.982975639701));
#4583=CARTESIAN_POINT('Ctrl Pts',(2.06964550137172,2.4706399525505,302.985232113078));
#4584=CARTESIAN_POINT('Ctrl Pts',(2.01288184600661,2.5170891350449,302.989731576848));
#4585=CARTESIAN_POINT('Ctrl Pts',(1.98444941896548,2.53956519435411,302.991973330519));
#4586=CARTESIAN_POINT('Ctrl Pts',(1.9136024405337,2.59365400375975,302.997533276792));
#4587=CARTESIAN_POINT('Ctrl Pts',(1.87077824453454,2.62471020010579,303.000871942451));
#4588=CARTESIAN_POINT('Ctrl Pts',(1.6663142656951,2.7654414522541,303.016719160653));
#4589=CARTESIAN_POINT('Ctrl Pts',(1.4957052382413,2.86131356461579,303.029711100135));
#4590=CARTESIAN_POINT('Ctrl Pts',(1.14465155149746,3.01856916110233,303.055622931002));
#4591=CARTESIAN_POINT('Ctrl Pts',(0.965309747860758,3.08061244993346,303.068476524314));
#4592=CARTESIAN_POINT('Ctrl Pts',(0.745898209242017,3.13545909671536,303.083106399989));
#4593=CARTESIAN_POINT('Ctrl Pts',(0.710096840959386,3.14376058577432,303.08545896521));
#4594=CARTESIAN_POINT('Ctrl Pts',(0.653102158562313,3.15595292155799,303.089141401667));
#4595=CARTESIAN_POINT('Ctrl Pts',(0.631999340417796,3.16024653579823,303.090491314491));
#4596=CARTESIAN_POINT('Ctrl Pts',(0.590095776164454,3.16833576443631,303.093142913525));
#4597=CARTESIAN_POINT('Ctrl Pts',(0.569297704291204,3.1721388227948,303.094444889453));
#4598=CARTESIAN_POINT('Ctrl Pts',(0.514131956612587,3.18166618002054,303.097864601036));
#4599=CARTESIAN_POINT('Ctrl Pts',(0.479705293320635,3.18703849991994,303.099964204537));
#4600=CARTESIAN_POINT('Ctrl Pts',(0.401777805202147,3.19790775962321,303.104652681084));
#4601=CARTESIAN_POINT('Ctrl Pts',(0.35823786897593,3.20307749029294,303.107227401044));
#4602=CARTESIAN_POINT('Ctrl Pts',(0.212352988394196,3.21738708739144,303.115744010839));
#4603=CARTESIAN_POINT('Ctrl Pts',(0.109674848605747,3.22252186847198,303.121558811112));
#4604=CARTESIAN_POINT('Ctrl Pts',(-0.231264026754964,3.22325415432443,303.140741777871));
#4605=CARTESIAN_POINT('Ctrl Pts',(-0.468751265253419,3.19736035322521,303.153962012385));
#4606=CARTESIAN_POINT('Ctrl Pts',(-0.754422865009971,3.13367767926094,303.171217721134));
#4607=CARTESIAN_POINT('Ctrl Pts',(-0.80732165319049,3.12046805758551,303.174468417191));
#4608=CARTESIAN_POINT('Ctrl Pts',(-0.891549973011353,3.09714991238025,303.179746952336));
#4609=CARTESIAN_POINT('Ctrl Pts',(-0.923105044203148,3.08789181975811,303.18174788583));
#4610=CARTESIAN_POINT('Ctrl Pts',(-0.988991136293969,3.06746103702494,303.185977874329));
#4611=CARTESIAN_POINT('Ctrl Pts',(-1.02328698497413,3.05619113650004,303.188209798947));
#4612=CARTESIAN_POINT('Ctrl Pts',(-1.10656455137934,3.02726656109742,303.193706300597));
#4613=CARTESIAN_POINT('Ctrl Pts',(-1.1553203326412,3.00899690495565,303.196990283259));
#4614=CARTESIAN_POINT('Ctrl Pts',(-1.3914325832045,2.91393691341763,303.213228028599));
#4615=CARTESIAN_POINT('Ctrl Pts',(-1.57168400618003,2.82079774467714,303.226708918506));
#4616=CARTESIAN_POINT('Ctrl Pts',(-1.89647521547669,2.6121291731121,303.252723428358));
#4617=CARTESIAN_POINT('Ctrl Pts',(-2.04221078422254,2.49984419389492,303.26517140535));
#4618=CARTESIAN_POINT('Ctrl Pts',(-2.20487479584916,2.35074753952906,303.279448856976));
#4619=CARTESIAN_POINT('Ctrl Pts',(-2.23172214386057,2.3252749076172,303.281818430088));
#4620=CARTESIAN_POINT('Ctrl Pts',(-2.2735276733419,2.28421878838031,303.28552103702));
#4621=CARTESIAN_POINT('Ctrl Pts',(-2.28877745225841,2.26893838386441,303.286874464034));
#4622=CARTESIAN_POINT('Ctrl Pts',(-2.31862457417345,2.23842415523771,303.289526868143));
#4623=CARTESIAN_POINT('Ctrl Pts',(-2.33322802772809,2.22319806325703,303.290826225489));
#4624=CARTESIAN_POINT('Ctrl Pts',(-2.37139441016025,2.18261408264355,303.294229903876));
#4625=CARTESIAN_POINT('Ctrl Pts',(-2.39470084180177,2.15701733309623,303.296316402392));
#4626=CARTESIAN_POINT('Ctrl Pts',(-2.44632778321765,2.09844859421542,303.300970002786));
#4627=CARTESIAN_POINT('Ctrl Pts',(-2.4744031209738,2.06526890475891,303.303523269194));
#4628=CARTESIAN_POINT('Ctrl Pts',(-2.5655817152442,1.95298378535035,303.311930437607));
#4629=CARTESIAN_POINT('Ctrl Pts',(-2.62563267707783,1.87147281167556,303.317660676606));
#4630=CARTESIAN_POINT('Ctrl Pts',(-2.81569372539025,1.58629080278081,303.336949523175));
#4631=CARTESIAN_POINT('Ctrl Pts',(-2.92660846150452,1.37091327505838,303.350344338374));
#4632=CARTESIAN_POINT('Ctrl Pts',(-3.03163722981131,1.09463097391607,303.367777357582));
#4633=CARTESIAN_POINT('Ctrl Pts',(-3.04957501095754,1.0436153599602,303.371002559855));
#4634=CARTESIAN_POINT('Ctrl Pts',(-3.07632202155272,0.960956303316408,303.376251042861));
#4635=CARTESIAN_POINT('Ctrl Pts',(-3.08594609560629,0.929586344529534,303.378248024955));
#4636=CARTESIAN_POINT('Ctrl Pts',(-3.10516834700565,0.863339612859892,303.382478743651));
#4637=CARTESIAN_POINT('Ctrl Pts',(-3.11466162469535,0.82843741352914,303.384715489576));
#4638=CARTESIAN_POINT('Ctrl Pts',(-3.13648284051657,0.742526935923535,303.390243232737));
#4639=CARTESIAN_POINT('Ctrl Pts',(-3.14815586945379,0.691364575490198,303.393554159819));
#4640=CARTESIAN_POINT('Ctrl Pts',(-3.19952951293693,0.437798800746816,303.410065432128));
#4641=CARTESIAN_POINT('Ctrl Pts',(-3.22097927321176,0.232219546214998,303.423813819264));
#4642=CARTESIAN_POINT('Ctrl Pts',(-3.22408194811515,-0.15186893454161,303.449704216477));
#4643=CARTESIAN_POINT('Ctrl Pts',(-3.21078554084386,-0.329595601194456,
303.46175161882));
#4644=CARTESIAN_POINT('Ctrl Pts',(-3.1769947099357,-0.542433264828102,303.475703594132));
#4645=CARTESIAN_POINT('Ctrl Pts',(-3.17045463772679,-0.579436707839862,
303.478110739751));
#4646=CARTESIAN_POINT('Ctrl Pts',(-3.15911805593236,-0.637621918302519,
303.481857872273));
#4647=CARTESIAN_POINT('Ctrl Pts',(-3.15475226010913,-0.658883025528071,
303.483219036873));
#4648=CARTESIAN_POINT('Ctrl Pts',(-3.1457400139075,-0.700627125412806,303.485873522869));
#4649=CARTESIAN_POINT('Ctrl Pts',(-3.14110752252592,-0.721111762154714,
303.487167420926));
#4650=CARTESIAN_POINT('Ctrl Pts',(-3.12841983970934,-0.774772414640497,
303.49053735861));
#4651=CARTESIAN_POINT('Ctrl Pts',(-3.12003692285038,-0.807869293173191,
303.492596223553));
#4652=CARTESIAN_POINT('Ctrl Pts',(-3.06806031743263,-1.00018675913143,303.504477624436));
#4653=CARTESIAN_POINT('Ctrl Pts',(-3.01280598652666,-1.15601884162136,303.513782491706));
#4654=CARTESIAN_POINT('Ctrl Pts',(-2.85829448932416,-1.50428718918191,303.535182829026));
#4655=CARTESIAN_POINT('Ctrl Pts',(-2.75114249946419,-1.69231587262444,303.547229867387));
#4656=CARTESIAN_POINT('Ctrl Pts',(-2.59296814802093,-1.91464909170332,303.563282079689));
#4657=CARTESIAN_POINT('Ctrl Pts',(-2.55870943262058,-1.96019652785262,303.56667392179));
#4658=CARTESIAN_POINT('Ctrl Pts',(-2.50025749546235,-2.03376439634545,303.572342092101));
#4659=CARTESIAN_POINT('Ctrl Pts',(-2.47675637025817,-2.06231977976725,303.574591597428));
#4660=CARTESIAN_POINT('Ctrl Pts',(-2.42919792277136,-2.11812076322277,303.579090524794));
#4661=CARTESIAN_POINT('Ctrl Pts',(-2.40516074822255,-2.14537635916619,303.581338943004));
#4662=CARTESIAN_POINT('Ctrl Pts',(-2.34464074878341,-2.21170395879428,303.586941404644));
#4663=CARTESIAN_POINT('Ctrl Pts',(-2.30763797041343,-2.25028467235845,303.590316642938));
#4664=CARTESIAN_POINT('Ctrl Pts',(-2.22503573099356,-2.33222870419721,303.597748933199));
#4665=CARTESIAN_POINT('Ctrl Pts',(-2.17909173714081,-2.37521222929232,303.601819436283));
#4666=CARTESIAN_POINT('Ctrl Pts',(-2.03076261350509,-2.506055998836,303.614762178431));
#4667=CARTESIAN_POINT('Ctrl Pts',(-1.9241084167384,-2.58884435303294,303.623791871355));
#4668=CARTESIAN_POINT('Ctrl Pts',(-1.70435177593856,-2.73832775044546,303.641700132459));
#4669=CARTESIAN_POINT('Ctrl Pts',(-1.59176505135959,-2.80526550205583,303.650554729941));
#4670=CARTESIAN_POINT('Ctrl Pts',(-1.47546383039573,-2.86515689757018,303.659226720281));
#4671=CARTESIAN_POINT('Origin',(0.,0.,294.689226550727));
#4672=CARTESIAN_POINT('',(-1.47546404664855,-2.86515678620691,305.155887179421));
#4673=CARTESIAN_POINT('',(-1.47546400239266,-2.86515680899727,304.907226776837));
#4674=CARTESIAN_POINT('',(-1.47546400239267,-2.86515680899727,294.689226550727));
#4675=CARTESIAN_POINT('Ctrl Pts',(-1.47546404664855,-2.86515678620691,305.155887179421));
#4676=CARTESIAN_POINT('Ctrl Pts',(-1.49316374364744,-2.85604200872452,305.154720915483));
#4677=CARTESIAN_POINT('Ctrl Pts',(-1.5107819037227,-2.8467617142584,305.153549744734));
#4678=CARTESIAN_POINT('Ctrl Pts',(-1.57449668637968,-2.81244184882883,305.149274969888));
#4679=CARTESIAN_POINT('Ctrl Pts',(-1.62006092853701,-2.78644416795494,305.146142369751));
#4680=CARTESIAN_POINT('Ctrl Pts',(-1.69591126983339,-2.74067666114335,305.140785984996));
#4681=CARTESIAN_POINT('Ctrl Pts',(-1.72653663150235,-2.72148758859424,305.138582960081));
#4682=CARTESIAN_POINT('Ctrl Pts',(-1.78430624294524,-2.68392302332692,305.134346362532));
#4683=CARTESIAN_POINT('Ctrl Pts',(-1.81150563956517,-2.66564040297228,305.132316372654));
#4684=CARTESIAN_POINT('Ctrl Pts',(-1.88274691770939,-2.61616020606856,305.126902653766));
#4685=CARTESIAN_POINT('Ctrl Pts',(-1.9262905287871,-2.5842667103688,305.123493416488));
#4686=CARTESIAN_POINT('Ctrl Pts',(-2.16072392027659,-2.40333834129658,305.104568210095));
#4687=CARTESIAN_POINT('Ctrl Pts',(-2.33512218897093,-2.23426314333312,305.0882725942));
#4688=CARTESIAN_POINT('Ctrl Pts',(-2.55302653029998,-1.96935467844235,305.065153258795));
#4689=CARTESIAN_POINT('Ctrl Pts',(-2.61344362514271,-1.88844289890856,305.058372279037));
#4690=CARTESIAN_POINT('Ctrl Pts',(-2.69426177257947,-1.7688847075046,305.048859923564));
#4691=CARTESIAN_POINT('Ctrl Pts',(-2.71783006194092,-1.7324548181515,305.046025233074));
#4692=CARTESIAN_POINT('Ctrl Pts',(-2.75884091741652,-1.66616594427883,305.040994526723));
#4693=CARTESIAN_POINT('Ctrl Pts',(-2.77655207708742,-1.63648126893127,305.038786177897));
#4694=CARTESIAN_POINT('Ctrl Pts',(-2.80428713421642,-1.58824911455079,305.035275759083));
#4695=CARTESIAN_POINT('Ctrl Pts',(-2.81461224766097,-1.56987883212058,305.03395652675));
#4696=CARTESIAN_POINT('Ctrl Pts',(-2.83513743179889,-1.53250719314596,305.031310546652));
#4697=CARTESIAN_POINT('Ctrl Pts',(-2.84532839740595,-1.51350220531433,305.029984333198));
#4698=CARTESIAN_POINT('Ctrl Pts',(-2.87246667299078,-1.46164935258219,305.026414336919));
#4699=CARTESIAN_POINT('Ctrl Pts',(-2.88904139628843,-1.42860900326692,305.024191679205));
#4700=CARTESIAN_POINT('Ctrl Pts',(-2.98495192823632,-1.22891966931751,305.011025125885));
#4701=CARTESIAN_POINT('Ctrl Pts',(-3.05042850666079,-1.05597453408301,305.000708662556));
#4702=CARTESIAN_POINT('Ctrl Pts',(-3.15575627952288,-0.684151336469236,
304.97901935552));
#4703=CARTESIAN_POINT('Ctrl Pts',(-3.19239832983542,-0.485224844343754,
304.967670947032));
#4704=CARTESIAN_POINT('Ctrl Pts',(-3.21477415564542,-0.232466607196427,
304.95267509705));
#4705=CARTESIAN_POINT('Ctrl Pts',(-3.21810202310599,-0.180644738732072,
304.949572888072));
#4706=CARTESIAN_POINT('Ctrl Pts',(-3.22161674848267,-0.0927493535312843,
304.944252604883));
#4707=CARTESIAN_POINT('Ctrl Pts',(-3.22245257605405,-0.0567111239931853,
304.942054610426));
#4708=CARTESIAN_POINT('Ctrl Pts',(-3.22289447443074,0.01219399505377,304.937817071601));
#4709=CARTESIAN_POINT('Ctrl Pts',(-3.22260257160361,0.045055828071636,304.935780931109));
#4710=CARTESIAN_POINT('Ctrl Pts',(-3.2204898432914,0.132427263979405,304.930324533378));
#4711=CARTESIAN_POINT('Ctrl Pts',(-3.21778783173552,0.186902957202241,304.926877996607));
#4712=CARTESIAN_POINT('Ctrl Pts',(-3.19589392540861,0.478514993889393,304.908179726014));
#4713=CARTESIAN_POINT('Ctrl Pts',(-3.15187114207106,0.713014122122916,304.892181500064));
#4714=CARTESIAN_POINT('Ctrl Pts',(-3.05243256585465,1.03892441235154,304.869211572598));
#4715=CARTESIAN_POINT('Ctrl Pts',(-3.01770073760766,1.13586647693936,304.862292821137));
#4716=CARTESIAN_POINT('Ctrl Pts',(-2.96163150045991,1.27152700900264,304.852613029857));
#4717=CARTESIAN_POINT('Ctrl Pts',(-2.94404801618804,1.31172546736024,304.84974538177));
#4718=CARTESIAN_POINT('Ctrl Pts',(-2.91103300150666,1.38319158874947,304.844663102886));
#4719=CARTESIAN_POINT('Ctrl Pts',(-2.89590459572361,1.41459142629879,304.842435785033));
#4720=CARTESIAN_POINT('Ctrl Pts',(-2.87079041445604,1.46462500581743,304.838902923953));
#4721=CARTESIAN_POINT('Ctrl Pts',(-2.86112584457242,1.4834159839704,304.837579844716));
#4722=CARTESIAN_POINT('Ctrl Pts',(-2.84125709313927,1.52113044032037,304.834933983126));
#4723=CARTESIAN_POINT('Ctrl Pts',(-2.8310470278782,1.54004950296656,304.83361161504));
#4724=CARTESIAN_POINT('Ctrl Pts',(-2.80292824391191,1.5909282924235,304.830064880375));
#4725=CARTESIAN_POINT('Ctrl Pts',(-2.78466216429091,1.62268803322388,304.827861168992));
#4726=CARTESIAN_POINT('Ctrl Pts',(-2.66798007151201,1.81779113570213,304.814344452143));
#4727=CARTESIAN_POINT('Ctrl Pts',(-2.55575840042095,1.97245970458257,304.803705390371));
#4728=CARTESIAN_POINT('Ctrl Pts',(-2.30290373160404,2.26285437228965,304.782092698221));
#4729=CARTESIAN_POINT('Ctrl Pts',(-2.16232317970976,2.39754544054297,304.771150909799));
#4730=CARTESIAN_POINT('Ctrl Pts',(-1.96919146406032,2.55170392376792,304.756559507566));
#4731=CARTESIAN_POINT('Ctrl Pts',(-1.92710459841531,2.58363606944183,304.753405726438));
#4732=CARTESIAN_POINT('Ctrl Pts',(-1.85488340600002,2.63568506461599,304.748024222789));
#4733=CARTESIAN_POINT('Ctrl Pts',(-1.82515951082132,2.65635479702645,304.745817740689));
#4734=CARTESIAN_POINT('Ctrl Pts',(-1.76430688753924,2.69716759318922,304.741313721397));
#4735=CARTESIAN_POINT('Ctrl Pts',(-1.73316623046602,2.7172829182394,304.739015612972));
#4736=CARTESIAN_POINT('Ctrl Pts',(-1.6527645920479,2.767273997165,304.733096008376));
#4737=CARTESIAN_POINT('Ctrl Pts',(-1.60303853246442,2.79637318172693,304.729447689896));
#4738=CARTESIAN_POINT('Ctrl Pts',(-1.37208669979633,2.92333897249458,304.712551974839));
#4739=CARTESIAN_POINT('Ctrl Pts',(-1.18254061012296,3.0050138347113,304.698777106955));
#4740=CARTESIAN_POINT('Ctrl Pts',(-0.872085231278484,3.10484082869179,304.676786954529));
#4741=CARTESIAN_POINT('Ctrl Pts',(-0.75566763338803,3.13520936077227,304.668670935858));
#4742=CARTESIAN_POINT('Ctrl Pts',(-0.590946363926448,3.16846758784061,304.657555009922));
#4743=CARTESIAN_POINT('Ctrl Pts',(-0.543863667735707,3.17688797338381,304.654419401677));
#4744=CARTESIAN_POINT('Ctrl Pts',(-0.459906743603022,3.18998168726016,304.648920527274));
#4745=CARTESIAN_POINT('Ctrl Pts',(-0.423106517064948,3.19507097248516,304.646541555823));
#4746=CARTESIAN_POINT('Ctrl Pts',(-0.364777809486342,3.20211202001002,304.6428286337));
#4747=CARTESIAN_POINT('Ctrl Pts',(-0.343304608254074,3.20448533248845,304.641474084295));
#4748=CARTESIAN_POINT('Ctrl Pts',(-0.30087268998837,3.20874366510589,304.638823880528));
#4749=CARTESIAN_POINT('Ctrl Pts',(-0.279916362748223,3.21063968000682,304.637527780647));
#4750=CARTESIAN_POINT('Ctrl Pts',(-0.224645954322845,3.21509496779267,304.634139632036));
#4751=CARTESIAN_POINT('Ctrl Pts',(-0.190305820533833,3.2173102683198,304.63206513669));
#4752=CARTESIAN_POINT('Ctrl Pts',(0.0548844912920111,3.22918790628011,304.61742992429));
#4753=CARTESIAN_POINT('Ctrl Pts',(0.26622330660073,3.21866637499759,304.605722496545));
#4754=CARTESIAN_POINT('Ctrl Pts',(0.641281462629434,3.16277212319044,304.58442108968));
#4755=CARTESIAN_POINT('Ctrl Pts',(0.805320483147841,3.12503139196682,304.574917732615));
#4756=CARTESIAN_POINT('Ctrl Pts',(1.02061127270893,3.05741519424331,304.561649176959));
#4757=CARTESIAN_POINT('Ctrl Pts',(1.0750871668516,3.0386875512137,304.558222437333));
#4758=CARTESIAN_POINT('Ctrl Pts',(1.16374926039165,3.00552479814698,304.552513792548));
#4759=CARTESIAN_POINT('Ctrl Pts',(1.19824099991222,2.99194083941493,304.550259593611));
#4760=CARTESIAN_POINT('Ctrl Pts',(1.26555320246021,2.96408048557714,304.545790559052));
#4761=CARTESIAN_POINT('Ctrl Pts',(1.29838538264591,2.9498463130635,304.543577383026));
#4762=CARTESIAN_POINT('Ctrl Pts',(1.37876990448207,2.91339415002311,304.538072902596));
#4763=CARTESIAN_POINT('Ctrl Pts',(1.42602812312218,2.8905562111598,304.534761254982));
#4764=CARTESIAN_POINT('Ctrl Pts',(1.69746549132284,2.75110503862986,304.515285323597));
#4765=CARTESIAN_POINT('Ctrl Pts',(1.90783311337018,2.60961688034789,304.498255595423));
#4766=CARTESIAN_POINT('Ctrl Pts',(2.17246739918002,2.38238481161996,304.474757591511));
#4767=CARTESIAN_POINT('Ctrl Pts',(2.24261382289641,2.31647511840793,304.468302749959));
#4768=CARTESIAN_POINT('Ctrl Pts',(2.33913904247339,2.21727916905321,304.45918885652));
#4769=CARTESIAN_POINT('Ctrl Pts',(2.36797323943586,2.18645864898127,304.456434207468));
#4770=CARTESIAN_POINT('Ctrl Pts',(2.41883679209558,2.12990435704553,304.451529156999));
#4771=CARTESIAN_POINT('Ctrl Pts',(2.44108150076025,2.10437290197028,304.449367263377));
#4772=CARTESIAN_POINT('Ctrl Pts',(2.4764199913087,2.06249841101479,304.445911814753));
#4773=CARTESIAN_POINT('Ctrl Pts',(2.48976373756538,2.04637051317138,304.444602002801));
#4774=CARTESIAN_POINT('Ctrl Pts',(2.51664464129725,2.01322873372171,304.441954944974));
#4775=CARTESIAN_POINT('Ctrl Pts',(2.53016853505408,1.99620575860901,304.440618541443));
#4776=CARTESIAN_POINT('Ctrl Pts',(2.56674258417041,1.94919988934794,304.436987430651));
#4777=CARTESIAN_POINT('Ctrl Pts',(2.58943956409225,1.91894520991004,304.434715094447));
#4778=CARTESIAN_POINT('Ctrl Pts',(2.74106846761206,1.70923556457782,304.419349333768));
#4779=CARTESIAN_POINT('Ctrl Pts',(2.85179303507868,1.51731383440288,304.407151278844));
#4780=CARTESIAN_POINT('Ctrl Pts',(2.99629973149484,1.19414882465384,304.387233964455));
#4781=CARTESIAN_POINT('Ctrl Pts',(3.04301688720277,1.06950826454934,304.379692200525));
#4782=CARTESIAN_POINT('Ctrl Pts',(3.10168370022079,0.877641101643442,304.367984795442));
#4783=CARTESIAN_POINT('Ctrl Pts',(3.11942458627493,0.812333067949683,304.363984693996));
#4784=CARTESIAN_POINT('Ctrl Pts',(3.14412273901258,0.708610093902216,304.357580362979));
#4785=CARTESIAN_POINT('Ctrl Pts',(3.15246067521097,0.670542732267735,304.355219305203));
#4786=CARTESIAN_POINT('Ctrl Pts',(3.16703610866834,0.597701700178213,304.350676781026));
#4787=CARTESIAN_POINT('Ctrl Pts',(3.17339612318629,0.562958193332626,304.34849950599));
#4788=CARTESIAN_POINT('Ctrl Pts',(3.18676820314149,0.482460500210809,304.343427616852));
#4789=CARTESIAN_POINT('Ctrl Pts',(3.19336797874565,0.436646675162563,304.340520730888));
#4790=CARTESIAN_POINT('Ctrl Pts',(3.21244026604963,0.280489707996374,304.330538429997));
#4791=CARTESIAN_POINT('Ctrl Pts',(3.22019535865749,0.169659834785927,304.323325110275));
#4792=CARTESIAN_POINT('Ctrl Pts',(3.22258796276283,0.0382331994695072,304.314634770256));
#4793=CARTESIAN_POINT('Ctrl Pts',(3.22276557763011,0.0178035706015105,304.313280132694));
#4794=CARTESIAN_POINT('Ctrl Pts',(3.22263452749977,-0.143019708263997,304.30258870143));
#4795=CARTESIAN_POINT('Ctrl Pts',(3.21334617871903,-0.283251278918383,304.293091111162));
#4796=CARTESIAN_POINT('Ctrl Pts',(3.1771700584407,-0.556864925498543,304.274507747648));
#4797=CARTESIAN_POINT('Ctrl Pts',(3.15092484735525,-0.690063204470942,304.265438596113));
#4798=CARTESIAN_POINT('Ctrl Pts',(3.10812548675147,-0.852477754685679,304.254626826507));
#4799=CARTESIAN_POINT('Ctrl Pts',(3.09941869919516,-0.883609796852329,304.252566198727));
#4800=CARTESIAN_POINT('Ctrl Pts',(3.08496537620158,-0.932444224090226,304.249358064959));
#4801=CARTESIAN_POINT('Ctrl Pts',(3.07953161619108,-0.95023611530413,304.24819435824));
#4802=CARTESIAN_POINT('Ctrl Pts',(3.06749714181303,-0.988453101375741,304.245707242786));
#4803=CARTESIAN_POINT('Ctrl Pts',(3.06084579618803,-1.00886139792871,304.244386806468));
#4804=CARTESIAN_POINT('Ctrl Pts',(3.04234348808644,-1.06376399127046,304.240851631853));
#4805=CARTESIAN_POINT('Ctrl Pts',(3.03010973815845,-1.09812701934421,304.238657318256));
#4806=CARTESIAN_POINT('Ctrl Pts',(3.00090570111415,-1.17595004655124,304.233714096154));
#4807=CARTESIAN_POINT('Ctrl Pts',(2.98356963825308,-1.21926459158721,304.230981786844));
#4808=CARTESIAN_POINT('Ctrl Pts',(2.92031969953649,-1.36785953148776,304.22162569127));
#4809=CARTESIAN_POINT('Ctrl Pts',(2.86972204020532,-1.47105577370453,304.215156659433));
#4810=CARTESIAN_POINT('Ctrl Pts',(2.70895547560288,-1.75893337525869,304.19663767952));
#4811=CARTESIAN_POINT('Ctrl Pts',(2.58570208625026,-1.93556758003063,304.184644633481));
#4812=CARTESIAN_POINT('Ctrl Pts',(2.40864786459496,-2.14191206046656,304.168650110785));
#4813=CARTESIAN_POINT('Ctrl Pts',(2.37035897601791,-2.18420913855521,304.165254878936));
#4814=CARTESIAN_POINT('Ctrl Pts',(2.30544259355637,-2.25220303101069,304.159584230742));
#4815=CARTESIAN_POINT('Ctrl Pts',(2.27945850618761,-2.2784979245228,304.157335746622));
#4816=CARTESIAN_POINT('Ctrl Pts',(2.22708560205572,-2.32970464415134,304.152841436414));
#4817=CARTESIAN_POINT('Ctrl Pts',(2.20071690282306,-2.3546292604049,304.150596655651));
#4818=CARTESIAN_POINT('Ctrl Pts',(2.13459837089485,-2.41504586990703,304.145008587956));
#4819=CARTESIAN_POINT('Ctrl Pts',(2.09437951490615,-2.45000626084511,304.141644296002));
#4820=CARTESIAN_POINT('Ctrl Pts',(2.00502239007602,-2.52387172156856,304.134239742906));
#4821=CARTESIAN_POINT('Ctrl Pts',(1.95557921687508,-2.56237241380963,304.130186191668));
#4822=CARTESIAN_POINT('Ctrl Pts',(1.79701268065843,-2.6785823674287,304.117324573989));
#4823=CARTESIAN_POINT('Ctrl Pts',(1.68415472921881,-2.75094089642649,304.108361225245));
#4824=CARTESIAN_POINT('Ctrl Pts',(1.40383780298862,-2.90693647913362,304.086747954692));
#4825=CARTESIAN_POINT('Ctrl Pts',(1.23293943748096,-2.98343921469679,304.074071436949));
#4826=CARTESIAN_POINT('Ctrl Pts',(1.02152704943106,-3.05678913817226,304.059593968997));
#4827=CARTESIAN_POINT('Ctrl Pts',(0.986482440994274,-3.06827801910034,304.05723288439));
#4828=CARTESIAN_POINT('Ctrl Pts',(0.930659950212072,-3.08552327545251,304.053541188323));
#4829=CARTESIAN_POINT('Ctrl Pts',(0.910009220843388,-3.09167674653208,304.052190348411));
#4830=CARTESIAN_POINT('Ctrl Pts',(0.869029013173711,-3.10344176922206,304.049541095819));
#4831=CARTESIAN_POINT('Ctrl Pts',(0.848703248760924,-3.10906176845595,304.048242331822));
#4832=CARTESIAN_POINT('Ctrl Pts',(0.794848170145396,-3.12338498990013,304.044837779364));
#4833=CARTESIAN_POINT('Ctrl Pts',(0.761230189213781,-3.13174810973855,304.042749860165));
#4834=CARTESIAN_POINT('Ctrl Pts',(0.685094696938178,-3.14938978324987,304.038091805848));
#4835=CARTESIAN_POINT('Ctrl Pts',(0.642510528896745,-3.15835262445451,304.035535558507));
#4836=CARTESIAN_POINT('Ctrl Pts',(0.500087224827143,-3.18532896403729,304.027110702863));
#4837=CARTESIAN_POINT('Ctrl Pts',(0.399576880784147,-3.19949189806946,304.021366354643));
#4838=CARTESIAN_POINT('Ctrl Pts',(0.058595382843254,-3.23121744376429,304.002093056539));
#4839=CARTESIAN_POINT('Ctrl Pts',(-0.183095845248976,-3.22655638666897,
303.988725313126));
#4840=CARTESIAN_POINT('Ctrl Pts',(-0.475657243538987,-3.1879141596626,303.971321021085));
#4841=CARTESIAN_POINT('Ctrl Pts',(-0.529121446324816,-3.17947739437225,
303.968093096521));
#4842=CARTESIAN_POINT('Ctrl Pts',(-0.614601548931674,-3.16377275658393,
303.962842894413));
#4843=CARTESIAN_POINT('Ctrl Pts',(-0.646764083781591,-3.15735478195386,
303.960847001965));
#4844=CARTESIAN_POINT('Ctrl Pts',(-0.714125520810718,-3.14284051298556,
303.956620892032));
#4845=CARTESIAN_POINT('Ctrl Pts',(-0.749297309101026,-3.13464114804011,
303.954387705999));
#4846=CARTESIAN_POINT('Ctrl Pts',(-0.835059302489682,-3.11312219198475,
303.948873958713));
#4847=CARTESIAN_POINT('Ctrl Pts',(-0.8854758371264,-3.09915889598517,303.945573647391));
#4848=CARTESIAN_POINT('Ctrl Pts',(-0.993997922765274,-3.06623857812937,
303.938337138034));
#4849=CARTESIAN_POINT('Ctrl Pts',(-1.05194844810441,-3.04684338497022,303.93438872369));
#4850=CARTESIAN_POINT('Ctrl Pts',(-1.22931376673303,-2.98181852584549,303.922045481515));
#4851=CARTESIAN_POINT('Ctrl Pts',(-1.34658497608694,-2.93072658628545,303.913509295283));
#4852=CARTESIAN_POINT('Ctrl Pts',(-1.46549794937883,-2.87027258315036,303.904529264724));
#4853=CARTESIAN_POINT('Ctrl Pts',(-1.47048445786938,-2.86772111497051,303.904152093631));
#4854=CARTESIAN_POINT('Ctrl Pts',(-1.47546400670695,-2.86515680677555,303.903774856397));
#4855=CARTESIAN_POINT('',(3.22274993609481,0.000641795043669797,304.064226550727));
#4856=CARTESIAN_POINT('Ctrl Pts',(-1.47546383039573,-2.86515689757018,303.659226720281));
#4857=CARTESIAN_POINT('Ctrl Pts',(-1.42721028503122,-2.89000592448876,303.662824741659));
#4858=CARTESIAN_POINT('Ctrl Pts',(-1.37831726698886,-2.9136420047774,303.666390446996));
#4859=CARTESIAN_POINT('Ctrl Pts',(-1.29516402843274,-2.95127654637207,303.672295924761));
#4860=CARTESIAN_POINT('Ctrl Pts',(-1.26123696973024,-2.96593403202772,303.674662149003));
#4861=CARTESIAN_POINT('Ctrl Pts',(-1.20711247731433,-2.98822063647225,303.678360785038));
#4862=CARTESIAN_POINT('Ctrl Pts',(-1.18707856567608,-2.99623557903244,303.679713520622));
#4863=CARTESIAN_POINT('Ctrl Pts',(-1.14729213728501,-3.0116911760669,303.682365758989));
#4864=CARTESIAN_POINT('Ctrl Pts',(-1.12754418368385,-3.01914013351242,303.68366562428));
#4865=CARTESIAN_POINT('Ctrl Pts',(-1.07517786037837,-3.03830730683537,303.687072420292));
#4866=CARTESIAN_POINT('Ctrl Pts',(-1.04244021666449,-3.04969462935961,303.689161468369));
#4867=CARTESIAN_POINT('Ctrl Pts',(-0.968182958571903,-3.07418840267462,
303.693821848812));
#4868=CARTESIAN_POINT('Ctrl Pts',(-0.926568233904473,-3.0869862672627,303.696379284248));
#4869=CARTESIAN_POINT('Ctrl Pts',(-0.78712094784443,-3.1267966028928,303.704807641956));
#4870=CARTESIAN_POINT('Ctrl Pts',(-0.688269642230302,-3.15003230638495,
303.71055424094));
#4871=CARTESIAN_POINT('Ctrl Pts',(-0.351661565381582,-3.21254885106674,
303.729822265074));
#4872=CARTESIAN_POINT('Ctrl Pts',(-0.110678289315643,-3.22984162327145,
303.743183048115));
#4873=CARTESIAN_POINT('Ctrl Pts',(0.184091553859675,-3.2179436110702,303.760581510385));
#4874=CARTESIAN_POINT('Ctrl Pts',(0.238140564724718,-3.21439564431528,303.7638117457));
#4875=CARTESIAN_POINT('Ctrl Pts',(0.324763550402713,-3.20651271082044,303.769066157839));
#4876=CARTESIAN_POINT('Ctrl Pts',(0.357406440570748,-3.20303850182447,303.771063916562));
#4877=CARTESIAN_POINT('Ctrl Pts',(0.425878714440959,-3.19469122883886,303.775294468203));
#4878=CARTESIAN_POINT('Ctrl Pts',(0.461690384211446,-3.18971261251982,303.7775302426));
#4879=CARTESIAN_POINT('Ctrl Pts',(0.549171294162807,-3.17604677324705,303.783051710502));
#4880=CARTESIAN_POINT('Ctrl Pts',(0.60072555925839,-3.16670025675986,303.786357228347));
#4881=CARTESIAN_POINT('Ctrl Pts',(0.848976813832634,-3.1154134170457,303.802533857509));
#4882=CARTESIAN_POINT('Ctrl Pts',(1.04165774162688,-3.05638505111758,303.815923010318));
#4883=CARTESIAN_POINT('Ctrl Pts',(1.3979614468484,-2.90960264591401,303.841889773519));
#4884=CARTESIAN_POINT('Ctrl Pts',(1.56204209193491,-2.82491010690087,303.854384928862));
#4885=CARTESIAN_POINT('Ctrl Pts',(1.74928030508781,-2.70693620975969,303.868704018369));
#4886=CARTESIAN_POINT('Ctrl Pts',(1.78022927902662,-2.68668368189604,303.871072134484));
#4887=CARTESIAN_POINT('Ctrl Pts',(1.82867739590745,-2.65377511119295,303.874773013877));
#4888=CARTESIAN_POINT('Ctrl Pts',(1.84640890386678,-2.6414688300028,303.876126140142));
#4889=CARTESIAN_POINT('Ctrl Pts',(1.8812286054825,-2.61678079157132,303.878778472229));
#4890=CARTESIAN_POINT('Ctrl Pts',(1.89832133571935,-2.60440759616097,303.880078050584));
#4891=CARTESIAN_POINT('Ctrl Pts',(1.9431449627143,-2.57128463172423,303.883483084594));
#4892=CARTESIAN_POINT('Ctrl Pts',(1.97066585772615,-2.55025357478157,303.885570691602));
#4893=CARTESIAN_POINT('Ctrl Pts',(2.03196857446068,-2.50182186425688,303.890227239359));
#4894=CARTESIAN_POINT('Ctrl Pts',(2.06554585056862,-2.47417250740885,303.892782317946));
#4895=CARTESIAN_POINT('Ctrl Pts',(2.17544385569904,-2.37987936369645,303.90119869178));
#4896=CARTESIAN_POINT('Ctrl Pts',(2.24918385394179,-2.3103151274614,303.906936037426));
#4897=CARTESIAN_POINT('Ctrl Pts',(2.48700622966486,-2.06376188313354,303.926215813664));
#4898=CARTESIAN_POINT('Ctrl Pts',(2.63444675915894,-1.87189582875144,303.939595825552));
#4899=CARTESIAN_POINT('Ctrl Pts',(2.78705964178637,-1.61905650342582,303.957013812769));
#4900=CARTESIAN_POINT('Ctrl Pts',(2.81384878923454,-1.57203686447769,303.960241207534));
#4901=CARTESIAN_POINT('Ctrl Pts',(2.85496367024925,-1.49545212041664,303.965492273484));
#4902=CARTESIAN_POINT('Ctrl Pts',(2.87004375258331,-1.46630260889329,303.967489594026));
#4903=CARTESIAN_POINT('Ctrl Pts',(2.90079951909344,-1.40455952313598,303.971720239599));
#4904=CARTESIAN_POINT('Ctrl Pts',(2.91637689450022,-1.37192235473578,303.973956561811));
#4905=CARTESIAN_POINT('Ctrl Pts',(2.95318807135371,-1.29133547228735,303.979481567271));
#4906=CARTESIAN_POINT('Ctrl Pts',(2.97380647823742,-1.24311769876269,303.982790134306));
#4907=CARTESIAN_POINT('Ctrl Pts',(3.06981177862278,-1.00252675031615,303.999321334109));
#4908=CARTESIAN_POINT('Ctrl Pts',(3.12774357035196,-0.803741738681032,304.01309427373));
#4909=CARTESIAN_POINT('Ctrl Pts',(3.1952597383578,-0.447935055643875,304.037505795203));
#4910=CARTESIAN_POINT('Ctrl Pts',(3.21316021117902,-0.293149978724763,304.048034960677));
#4911=CARTESIAN_POINT('Ctrl Pts',(3.22177552726619,-0.0916576274483147,
304.061238275884));
#4912=CARTESIAN_POINT('Ctrl Pts',(3.22275646548227,-0.045605109878821,304.064221202948));
#4913=CARTESIAN_POINT('Ctrl Pts',(3.22274996793341,0.000454626470845607,
304.067160013823));
#4914=CARTESIAN_POINT('Ctrl Pts',(3.22274993609481,0.000641795043669797,
304.064226550727));
#4915=CARTESIAN_POINT('Ctrl Pts',(3.22274270887017,0.0369330347259519,304.066479769874));
#4916=CARTESIAN_POINT('Ctrl Pts',(3.2221224892191,0.0732173351279854,304.068732989021));
#4917=CARTESIAN_POINT('Ctrl Pts',(3.22088986744413,0.109480702846282,304.070986208168));
#4918=CARTESIAN_POINT('Ctrl Pts',(3.21750812042288,0.208970699090797,304.077168004802));
#4919=CARTESIAN_POINT('Ctrl Pts',(3.20950662367668,0.308472350520246,304.083349801435));
#4920=CARTESIAN_POINT('Ctrl Pts',(3.19688017044917,0.407522684385618,304.089531598069));
#4921=CARTESIAN_POINT('Ctrl Pts',(3.18427039939254,0.506442152158601,304.095705227263));
#4922=CARTESIAN_POINT('Ctrl Pts',(3.16704787283313,0.604911061938199,304.101878856457));
#4923=CARTESIAN_POINT('Ctrl Pts',(3.14525937378961,0.702467817119461,304.108052485652));
#4924=CARTESIAN_POINT('Ctrl Pts',(3.12349328461099,0.799924233415559,304.114219765157));
#4925=CARTESIAN_POINT('Ctrl Pts',(3.09717065431162,0.89646994031363,304.120387044662));
#4926=CARTESIAN_POINT('Ctrl Pts',(3.06638978326791,0.991650775006099,304.126554324167));
#4927=CARTESIAN_POINT('Ctrl Pts',(3.03563043930724,1.08676504349487,304.132717290489));
#4928=CARTESIAN_POINT('Ctrl Pts',(3.00041918691307,1.18051592712785,304.138880256811));
#4929=CARTESIAN_POINT('Ctrl Pts',(2.96090467180656,1.27246260729898,304.145043223133));
#4930=CARTESIAN_POINT('Ctrl Pts',(2.92140428172553,1.36437641982142,304.151203986415));
#4931=CARTESIAN_POINT('Ctrl Pts',(2.87760385661249,1.45448691337522,304.157364749697));
#4932=CARTESIAN_POINT('Ctrl Pts',(2.82970054147019,1.54237233121686,304.163525512979));
#4933=CARTESIAN_POINT('Ctrl Pts',(2.78180165436517,1.63024962519682,304.169685706779));
#4934=CARTESIAN_POINT('Ctrl Pts',(2.72980083863594,1.7159018725651,304.175845900578));
#4935=CARTESIAN_POINT('Ctrl Pts',(2.67394118373631,1.79893193546028,304.182006094378));
#4936=CARTESIAN_POINT('Ctrl Pts',(2.61807188827152,1.88197632813843,304.188167351338));
#4937=CARTESIAN_POINT('Ctrl Pts',(2.5583426722861,1.96239727833134,304.194328608297));
#4938=CARTESIAN_POINT('Ctrl Pts',(2.49503936435757,2.03982747623572,304.200489865257));
#4939=CARTESIAN_POINT('Ctrl Pts',(2.43166966342175,2.11733888354072,304.206657584192));
#4940=CARTESIAN_POINT('Ctrl Pts',(2.36471866053422,2.19185294013554,304.212825303126));
#4941=CARTESIAN_POINT('Ctrl Pts',(2.2945117214989,2.26303635021715,304.21899302206));
#4942=CARTESIAN_POINT('Ctrl Pts',(2.22426479073441,2.33426030825166,304.225164254291));
#4943=CARTESIAN_POINT('Ctrl Pts',(2.1507585479264,2.40214954778274,304.231335486521));
#4944=CARTESIAN_POINT('Ctrl Pts',(2.07435286996306,2.46640988754425,304.237506718751));
#4945=CARTESIAN_POINT('Ctrl Pts',(1.99782617432783,2.53077200818016,304.243687725493));
#4946=CARTESIAN_POINT('Ctrl Pts',(1.91839121605936,2.59149348779603,304.249868732234));
#4947=CARTESIAN_POINT('Ctrl Pts',(1.8364383890743,2.64832241345993,304.256049738976));
#4948=CARTESIAN_POINT('Ctrl Pts',(1.78626370496904,2.6831152753797,304.259833989893));
#4949=CARTESIAN_POINT('Ctrl Pts',(1.73514577394337,2.71644993843564,304.263618240811));
#4950=CARTESIAN_POINT('Ctrl Pts',(1.68317857908835,2.74827717550435,304.267402491728));
#4951=CARTESIAN_POINT('Ctrl Pts',(1.59828709345055,2.800268849214,304.273584289366));
#4952=CARTESIAN_POINT('Ctrl Pts',(1.5108406362507,2.84841158071823,304.279766087004));
#4953=CARTESIAN_POINT('Ctrl Pts',(1.42122270787832,2.89244595059458,304.285947884642));
#4954=CARTESIAN_POINT('Ctrl Pts',(1.33172318347992,2.93642214188458,304.292121514836));
#4955=CARTESIAN_POINT('Ctrl Pts',(1.24005827613208,2.97630057223439,304.29829514503));
#4956=CARTESIAN_POINT('Ctrl Pts',(1.14663898146327,3.01186596791572,304.304468775224));
#4957=CARTESIAN_POINT('Ctrl Pts',(1.05331577030405,3.04739478391563,304.310636055723));
#4958=CARTESIAN_POINT('Ctrl Pts',(0.958242161946662,3.0786192323306,304.316803336222));
#4959=CARTESIAN_POINT('Ctrl Pts',(0.861851331633066,3.10537112832948,304.322970616721));
#4960=CARTESIAN_POINT('Ctrl Pts',(0.76552791394728,3.13210431491791,304.329133584023));
#4961=CARTESIAN_POINT('Ctrl Pts',(0.667889521836277,3.15437105312516,304.335296551325));
#4962=CARTESIAN_POINT('Ctrl Pts',(0.569385931973019,3.17205252525415,304.341459518628));
#4963=CARTESIAN_POINT('Ctrl Pts',(0.470917553749367,3.18972767686604,304.347620282881));
#4964=CARTESIAN_POINT('Ctrl Pts',(0.371585017917073,3.20282074334881,304.353781047135));
#4965=CARTESIAN_POINT('Ctrl Pts',(0.271848913885091,3.21126388366318,304.359941811389));
#4966=CARTESIAN_POINT('Ctrl Pts',(0.172122029311349,3.21970624350611,304.366102006151));
#4967=CARTESIAN_POINT('Ctrl Pts',(0.071992081938208,3.2234994955584,304.372262200913));
#4968=CARTESIAN_POINT('Ctrl Pts',(-0.0280755712182601,3.22262770496388,
304.378422395675));
#4969=CARTESIAN_POINT('Ctrl Pts',(-0.128160494419948,3.22175576391252,304.384583653586));
#4970=CARTESIAN_POINT('Ctrl Pts',(-0.228182669313109,3.21621718470132,304.390744911497));
#4971=CARTESIAN_POINT('Ctrl Pts',(-0.327678084504641,3.20604813367413,304.396906169408));
#4972=CARTESIAN_POINT('Ctrl Pts',(-0.427277850894759,3.19586841730461,304.403073889272));
#4973=CARTESIAN_POINT('Ctrl Pts',(-0.526349323288656,3.18104857672552,304.409241609135));
#4974=CARTESIAN_POINT('Ctrl Pts',(-0.624435093329909,3.16167651361079,304.415409328999));
#4975=CARTESIAN_POINT('Ctrl Pts',(-0.722576735433399,3.14229341569339,304.421580562147));
#4976=CARTESIAN_POINT('Ctrl Pts',(-0.819731136896843,3.11835303448159,304.427751795295));
#4977=CARTESIAN_POINT('Ctrl Pts',(-0.915454518139479,3.08999362260151,304.433923028444));
#4978=CARTESIAN_POINT('Ctrl Pts',(-1.0113295136034,3.06158929285401,304.440104036076));
#4979=CARTESIAN_POINT('Ctrl Pts',(-1.10576855380984,3.02875209677308,304.446285043709));
#4980=CARTESIAN_POINT('Ctrl Pts',(-1.19834632044172,2.99166904232133,304.452466051342));
#4981=CARTESIAN_POINT('Ctrl Pts',(-1.25502585073748,2.96896542584055,304.456250292657));
#4982=CARTESIAN_POINT('Ctrl Pts',(-1.31100814087214,2.94467124833667,304.460034533973));
#4983=CARTESIAN_POINT('Ctrl Pts',(-1.3662003297416,2.91883782035144,304.463818775288));
#4984=CARTESIAN_POINT('Ctrl Pts',(-1.45636028043439,2.87663727275434,304.470000574151));
#4985=CARTESIAN_POINT('Ctrl Pts',(-1.54471579429518,2.83018393049281,304.476182373015));
#4986=CARTESIAN_POINT('Ctrl Pts',(-1.63083908656621,2.77965491315521,304.482364171878));
#4987=CARTESIAN_POINT('Ctrl Pts',(-1.71684859223722,2.72919265505235,304.488537803312));
#4988=CARTESIAN_POINT('Ctrl Pts',(-1.8006313687029,2.67466564314972,304.494711434746));
#4989=CARTESIAN_POINT('Ctrl Pts',(-1.88178132407699,2.61629826488783,304.50088506618));
#4990=CARTESIAN_POINT('Ctrl Pts',(-1.96284781537727,2.55799091844166,304.507052347932));
#4991=CARTESIAN_POINT('Ctrl Pts',(-2.04128652024617,2.49585131065189,304.513219629684));
#4992=CARTESIAN_POINT('Ctrl Pts',(-2.11671842451974,2.43014828226565,304.519386911436));
#4993=CARTESIAN_POINT('Ctrl Pts',(-2.19209757434309,2.36449120429222,304.525549880006));
#4994=CARTESIAN_POINT('Ctrl Pts',(-2.26447377934179,2.29527594436833,304.531712848575));
#4995=CARTESIAN_POINT('Ctrl Pts',(-2.33350007763975,2.22281239652726,304.537875817145));
#4996=CARTESIAN_POINT('Ctrl Pts',(-2.40250170151066,2.15037475180673,304.544036582674));
#4997=CARTESIAN_POINT('Ctrl Pts',(-2.46815550023419,2.0746914397404,304.550197348203));
#4998=CARTESIAN_POINT('Ctrl Pts',(-2.53015109670326,1.99610946351929,304.556358113733));
#4999=CARTESIAN_POINT('Ctrl Pts',(-2.59214096245767,1.91753475121545,304.562518309777));
#5000=CARTESIAN_POINT('Ctrl Pts',(-2.65047303046909,1.836062247411,304.56867850582));
#5001=CARTESIAN_POINT('Ctrl Pts',(-2.70487761467672,1.75207153167922,304.574838701864));
#5002=CARTESIAN_POINT('Ctrl Pts',(-2.75929158826951,1.66806632045609,304.580999961062));
#5003=CARTESIAN_POINT('Ctrl Pts',(-2.80977649635269,1.58154239721343,304.58716122026));
#5004=CARTESIAN_POINT('Ctrl Pts',(-2.85610687473354,1.49290692362244,304.593322479458));
#5005=CARTESIAN_POINT('Ctrl Pts',(-2.90248584459074,1.40417848881099,304.599490200608));
#5006=CARTESIAN_POINT('Ctrl Pts',(-2.94470138412596,1.31333446610857,304.605657921758));
#5007=CARTESIAN_POINT('Ctrl Pts',(-2.98257484224445,1.22080501019225,304.611825642907));
#5008=CARTESIAN_POINT('Ctrl Pts',(-3.02046987401923,1.12822284721463,304.617996877343));
#5009=CARTESIAN_POINT('Ctrl Pts',(-3.0540177534552,1.03395374656585,304.624168111779));
#5010=CARTESIAN_POINT('Ctrl Pts',(-3.08308935805661,0.938444229956196,304.630339346215));
#5011=CARTESIAN_POINT('Ctrl Pts',(-3.11220700849388,0.84278343805284,304.636520355126));
#5012=CARTESIAN_POINT('Ctrl Pts',(-3.13683411875208,0.745878725935652,304.642701364036));
#5013=CARTESIAN_POINT('Ctrl Pts',(-3.15689242578227,0.648188070345756,304.648882372946));
#5014=CARTESIAN_POINT('Ctrl Pts',(-3.16917281898703,0.588378453249517,304.65266660158));
#5015=CARTESIAN_POINT('Ctrl Pts',(-3.17974169464408,0.528274395310344,304.656450830215));
#5016=CARTESIAN_POINT('Ctrl Pts',(-3.18859071179392,0.467981661138088,304.660235058849));
#5017=CARTESIAN_POINT('Ctrl Pts',(-3.20304617518148,0.369489433514989,304.666416850289));
#5018=CARTESIAN_POINT('Ctrl Pts',(-3.21295837398269,0.270160007624854,304.67259864173));
#5019=CARTESIAN_POINT('Ctrl Pts',(-3.21823943364067,0.170447969363531,304.67878043317));
#5020=CARTESIAN_POINT('Ctrl Pts',(-3.22351351591203,0.0708676716027387,
304.684954057169));
#5021=CARTESIAN_POINT('Ctrl Pts',(-3.22416859929969,-0.029093805070177,
304.691127681167));
#5022=CARTESIAN_POINT('Ctrl Pts',(-3.22016820776668,-0.128973936083073,
304.697301305165));
#5023=CARTESIAN_POINT('Ctrl Pts',(-3.21617193070947,-0.22875133855581,304.703468579478));
#5024=CARTESIAN_POINT('Ctrl Pts',(-3.2075297165177,-0.328447131537302,304.709635853792));
#5025=CARTESIAN_POINT('Ctrl Pts',(-3.19425710561108,-0.427596896332428,
304.715803128105));
#5026=CARTESIAN_POINT('Ctrl Pts',(-3.18099377706077,-0.526677319575138,
304.721966089262));
#5027=CARTESIAN_POINT('Ctrl Pts',(-3.16310654793605,-0.625212046189163,
304.72812905042));
#5028=CARTESIAN_POINT('Ctrl Pts',(-3.1406628783991,-0.722740788074029,304.734292011577));
#5029=CARTESIAN_POINT('Ctrl Pts',(-3.11822723160842,-0.820234667195105,
304.740452769714));
#5030=CARTESIAN_POINT('Ctrl Pts',(-3.09123847817242,-0.916722854915224,
304.74661352785));
#5031=CARTESIAN_POINT('Ctrl Pts',(-3.05981520363205,-1.01175514929361,304.752774285987));
#5032=CARTESIAN_POINT('Ctrl Pts',(-3.02839483363719,-1.10677865955807,304.758934474667));
#5033=CARTESIAN_POINT('Ctrl Pts',(-2.99254089362575,-1.20034613325871,304.765094663346));
#5034=CARTESIAN_POINT('Ctrl Pts',(-2.95242157408443,-1.29202337880583,304.771254852026));
#5035=CARTESIAN_POINT('Ctrl Pts',(-2.91229533031941,-1.38371644699806,304.777416103897));
#5036=CARTESIAN_POINT('Ctrl Pts',(-2.8679024181892,-1.47351824254347,304.783577355768));
#5037=CARTESIAN_POINT('Ctrl Pts',(-2.81945841049582,-1.56101628242129,304.78973860764));
#5038=CARTESIAN_POINT('Ctrl Pts',(-2.7709635936813,-1.64860609213236,304.795906321565));
#5039=CARTESIAN_POINT('Ctrl Pts',(-2.71840940790595,-1.73388694266899,304.80207403549));
#5040=CARTESIAN_POINT('Ctrl Pts',(-2.66205640614232,-1.81647275041952,304.808241749415));
#5041=CARTESIAN_POINT('Ctrl Pts',(-2.60567130385045,-1.89910560176969,304.814412976674));
#5042=CARTESIAN_POINT('Ctrl Pts',(-2.5454833361712,-1.97904000729206,304.820584203932));
#5043=CARTESIAN_POINT('Ctrl Pts',(-2.48179400269614,-2.0559221995692,304.826755431191));
#5044=CARTESIAN_POINT('Ctrl Pts',(-2.418003791556,-2.13292616570736,304.832936433068));
#5045=CARTESIAN_POINT('Ctrl Pts',(-2.35070143055836,-2.20686794414452,304.839117434946));
#5046=CARTESIAN_POINT('Ctrl Pts',(-2.28022599988325,-2.27742990055817,304.845298436824));
#5047=CARTESIAN_POINT('Ctrl Pts',(-2.23707760601933,-2.32063126957402,304.849082738686));
#5048=CARTESIAN_POINT('Ctrl Pts',(-2.19274048532147,-2.36256648331417,304.852867040547));
#5049=CARTESIAN_POINT('Ctrl Pts',(-2.14729831213303,-2.40317030632676,304.856651342409));
#5050=CARTESIAN_POINT('Ctrl Pts',(-2.07306817973536,-2.46949695724588,304.862833028022));
#5051=CARTESIAN_POINT('Ctrl Pts',(-1.99563638067943,-2.53249344176403,304.869014713635));
#5052=CARTESIAN_POINT('Ctrl Pts',(-1.91533385259366,-2.59183598933434,304.875196399248));
#5053=CARTESIAN_POINT('Ctrl Pts',(-1.83514776257405,-2.65109249065375,304.881369121463));
#5054=CARTESIAN_POINT('Ctrl Pts',(-1.75209956719673,-2.7067053372349,304.887541843678));
#5055=CARTESIAN_POINT('Ctrl Pts',(-1.66655500082802,-2.75838938362863,304.893714565893));
#5056=CARTESIAN_POINT('Ctrl Pts',(-1.60413541858516,-2.79610185002436,304.898218636207));
#5057=CARTESIAN_POINT('Ctrl Pts',(-1.54038748697828,-2.83172329355576,304.902722706522));
#5058=CARTESIAN_POINT('Ctrl Pts',(-1.47546400239266,-2.86515680899727,304.907226776837));
#5059=CARTESIAN_POINT('Origin',(0.,0.,294.689226550727));
#5060=CARTESIAN_POINT('',(-1.47546400239267,-2.86515680899727,306.403639991207));
#5061=CARTESIAN_POINT('',(-1.47546400238963,-2.86515680899883,306.154894777109));
#5062=CARTESIAN_POINT('',(-1.47546400239267,-2.86515680899727,294.689226550727));
#5063=CARTESIAN_POINT('',(3.22274909182747,0.00241942662847882,305.560773449333));
#5064=CARTESIAN_POINT('Ctrl Pts',(3.22274909182747,0.00241942662847882,
305.560773449333));
#5065=CARTESIAN_POINT('Ctrl Pts',(3.22266144451175,0.119168289285173,305.567961004005));
#5066=CARTESIAN_POINT('Ctrl Pts',(3.21622575765141,0.235660092573957,305.575148558678));
#5067=CARTESIAN_POINT('Ctrl Pts',(3.20354916784432,0.351269542807173,305.58233611335));
#5068=CARTESIAN_POINT('Ctrl Pts',(3.19074689796521,0.468025184899005,305.589594927912));
#5069=CARTESIAN_POINT('Ctrl Pts',(3.17157944877209,0.583880777920902,305.596853742474));
#5070=CARTESIAN_POINT('Ctrl Pts',(3.14620685056165,0.69821201363122,305.604112557036));
#5071=CARTESIAN_POINT('Ctrl Pts',(3.12176984277167,0.8083273937952,305.611103709717));
#5072=CARTESIAN_POINT('Ctrl Pts',(3.09157724993706,0.917028816844444,305.618094862397));
#5073=CARTESIAN_POINT('Ctrl Pts',(3.05581386047934,1.02377693498258,305.625086015078));
#5074=CARTESIAN_POINT('Ctrl Pts',(3.02418624482621,1.11818041584281,305.631268692204));
#5075=CARTESIAN_POINT('Ctrl Pts',(2.98812642735059,1.21127659330337,305.637451369331));
#5076=CARTESIAN_POINT('Ctrl Pts',(2.94776157123372,1.30262016016095,305.643634046457));
#5077=CARTESIAN_POINT('Ctrl Pts',(2.90745005343074,1.39384302519247,305.649808553764));
#5078=CARTESIAN_POINT('Ctrl Pts',(2.86284497866514,1.48331749083947,305.655983061071));
#5079=CARTESIAN_POINT('Ctrl Pts',(2.81412294498844,1.57061440620848,305.662157568379));
#5080=CARTESIAN_POINT('Ctrl Pts',(2.76545104354432,1.65782149796103,305.668325722465));
#5081=CARTESIAN_POINT('Ctrl Pts',(2.71267081576087,1.74285511862323,305.674493876552));
#5082=CARTESIAN_POINT('Ctrl Pts',(2.65600611370655,1.82530794291085,305.680662030638));
#5083=CARTESIAN_POINT('Ctrl Pts',(2.59938111668075,1.90770299240003,305.686825862691));
#5084=CARTESIAN_POINT('Ctrl Pts',(2.53887730176894,1.9875204856622,305.692989694744));
#5085=CARTESIAN_POINT('Ctrl Pts',(2.47476296555049,2.06438025248251,305.699153526797));
#5086=CARTESIAN_POINT('Ctrl Pts',(2.41067160505096,2.14121247618996,305.705315150008));
#5087=CARTESIAN_POINT('Ctrl Pts',(2.34297257137275,2.21508874797334,305.711476773218));
#5088=CARTESIAN_POINT('Ctrl Pts',(2.27197520644782,2.28566100368938,305.717638396429));
#5089=CARTESIAN_POINT('Ctrl Pts',(2.20098448217963,2.3562266585108,305.723799443319));
#5090=CARTESIAN_POINT('Ctrl Pts',(2.12669634706602,2.42348860692162,305.729960490209));
#5091=CARTESIAN_POINT('Ctrl Pts',(2.04945715566873,2.48713548677555,305.736121537099));
#5092=CARTESIAN_POINT('Ctrl Pts',(1.97220473453455,2.55079326823861,305.74228363927));
#5093=CARTESIAN_POINT('Ctrl Pts',(1.892000586925,2.61083447604423,305.748445741441));
#5094=CARTESIAN_POINT('Ctrl Pts',(1.80922352338026,2.66698852733707,305.754607843612));
#5095=CARTESIAN_POINT('Ctrl Pts',(1.72635988471605,2.72320130919476,305.760776390621));
#5096=CARTESIAN_POINT('Ctrl Pts',(1.64091831588962,2.77551857399083,305.766944937629));
#5097=CARTESIAN_POINT('Ctrl Pts',(1.55330582060207,2.82371361688535,305.773113484638));
#5098=CARTESIAN_POINT('Ctrl Pts',(1.46564354584226,2.8719360431319,305.779285536477));
#5099=CARTESIAN_POINT('Ctrl Pts',(1.37580827627961,2.91603139226436,305.785457588317));
#5100=CARTESIAN_POINT('Ctrl Pts',(1.28422894017585,2.95582029083549,305.791629640157));
#5101=CARTESIAN_POINT('Ctrl Pts',(1.19250489049869,2.99567206378351,305.797811445067));
#5102=CARTESIAN_POINT('Ctrl Pts',(1.09903167471182,3.03120364246141,305.803993249977));
#5103=CARTESIAN_POINT('Ctrl Pts',(1.00425541741988,3.06228486902881,305.810175054887));
#5104=CARTESIAN_POINT('Ctrl Pts',(0.946367589946561,3.08126878686438,305.813950802804));
#5105=CARTESIAN_POINT('Ctrl Pts',(0.887993923017348,3.09859345610937,305.817726550721));
#5106=CARTESIAN_POINT('Ctrl Pts',(0.829237818619394,3.11423862327076,305.821502298639));
#5107=CARTESIAN_POINT('Ctrl Pts',(0.73303586325626,3.13985461140222,305.827684368338));
#5108=CARTESIAN_POINT('Ctrl Pts',(0.635483189190926,3.16105208401201,305.833866438036));
#5109=CARTESIAN_POINT('Ctrl Pts',(0.537021435084952,3.17769185742723,305.840048507735));
#5110=CARTESIAN_POINT('Ctrl Pts',(0.438689601616051,3.19430967460185,305.846222420171));
#5111=CARTESIAN_POINT('Ctrl Pts',(0.339451495731243,3.20638167574098,305.852396332606));
#5112=CARTESIAN_POINT('Ctrl Pts',(0.239762506137257,3.21381883483665,305.858570245042));
#5113=CARTESIAN_POINT('Ctrl Pts',(0.140175888083489,3.22124835664525,305.86473781743));
#5114=CARTESIAN_POINT('Ctrl Pts',(0.0401397362372681,3.2240524679527,305.870905389818));
#5115=CARTESIAN_POINT('Ctrl Pts',(-0.0598827445386845,3.22219360365055,
305.877072962207));
#5116=CARTESIAN_POINT('Ctrl Pts',(-0.159835487309292,3.22033603539193,305.88323623442));
#5117=CARTESIAN_POINT('Ctrl Pts',(-0.259774146540478,3.21382196388716,305.889399506633));
#5118=CARTESIAN_POINT('Ctrl Pts',(-0.359233696008545,3.20266587613383,305.895562778846));
#5119=CARTESIAN_POINT('Ctrl Pts',(-0.458657821243816,3.19151376181343,305.901723855903));
#5120=CARTESIAN_POINT('Ctrl Pts',(-0.557602746265318,3.17572296510507,305.90788493296));
#5121=CARTESIAN_POINT('Ctrl Pts',(-0.655607631094898,3.15535991553264,305.914046010018));
#5122=CARTESIAN_POINT('Ctrl Pts',(-0.753603575423269,3.13499872358057,305.92020652503));
#5123=CARTESIAN_POINT('Ctrl Pts',(-0.850659226471839,3.1100661963613,305.926367040043));
#5124=CARTESIAN_POINT('Ctrl Pts',(-0.946323988758447,3.08067987152192,305.932527555056));
#5125=CARTESIAN_POINT('Ctrl Pts',(-1.04200536918741,3.05128844191754,305.938689140225));
#5126=CARTESIAN_POINT('Ctrl Pts',(-1.13629496728062,3.01744180488538,305.944850725395));
#5127=CARTESIAN_POINT('Ctrl Pts',(-1.22875834596989,2.97930704857847,305.951012310565));
#5128=CARTESIAN_POINT('Ctrl Pts',(-1.32131882448577,2.94113224530076,305.957180366284));
#5129=CARTESIAN_POINT('Ctrl Pts',(-1.41204885382933,2.89866049697703,305.963348422003));
#5130=CARTESIAN_POINT('Ctrl Pts',(-1.50053508857693,2.85210659170541,305.969516477722));
#5131=CARTESIAN_POINT('Ctrl Pts',(-1.58907180069417,2.80552612954964,305.975688052036));
#5132=CARTESIAN_POINT('Ctrl Pts',(-1.67536179601707,2.75485909172001,305.98185962635));
#5133=CARTESIAN_POINT('Ctrl Pts',(-1.75901915928313,2.70036463459564,305.988031200664));
#5134=CARTESIAN_POINT('Ctrl Pts',(-1.84280908563422,2.64578382579737,305.994212554427));
#5135=CARTESIAN_POINT('Ctrl Pts',(-1.92395769789876,2.58736373851854,306.000393908191));
#5136=CARTESIAN_POINT('Ctrl Pts',(-2.00211068653864,2.52540498957054,306.006575261954));
#5137=CARTESIAN_POINT('Ctrl Pts',(-2.04991652391241,2.48750509696709,306.010356368702));
#5138=CARTESIAN_POINT('Ctrl Pts',(-2.09660216060085,2.44828190783947,306.014137475451));
#5139=CARTESIAN_POINT('Ctrl Pts',(-2.14209342392823,2.4078108990665,306.017918582199));
#5140=CARTESIAN_POINT('Ctrl Pts',(-2.21641229141797,2.34169359833276,306.024095758888));
#5141=CARTESIAN_POINT('Ctrl Pts',(-2.2877942136428,2.27201918274831,306.030272935578));
#5142=CARTESIAN_POINT('Ctrl Pts',(-2.35587991540464,2.19907875863804,306.036450112267));
#5143=CARTESIAN_POINT('Ctrl Pts',(-2.42387544698635,2.12623493412226,306.042619108133));
#5144=CARTESIAN_POINT('Ctrl Pts',(-2.48858314210488,2.05013401311274,306.048788103999));
#5145=CARTESIAN_POINT('Ctrl Pts',(-2.5496779625577,1.97110625024316,306.054957099864));
#5146=CARTESIAN_POINT('Ctrl Pts',(-2.61070982913654,1.89215991987125,306.061119739018));
#5147=CARTESIAN_POINT('Ctrl Pts',(-2.66813595915531,1.81029308516022,306.067282378171));
#5148=CARTESIAN_POINT('Ctrl Pts',(-2.72166992036475,1.72587091263562,306.073445017324));
#5149=CARTESIAN_POINT('Ctrl Pts',(-2.77516648941635,1.64150770692628,306.079603352026));
#5150=CARTESIAN_POINT('Ctrl Pts',(-2.82477606335493,1.55459307714627,306.085761686727));
#5151=CARTESIAN_POINT('Ctrl Pts',(-2.87025462220028,1.46552242092638,306.091920021428));
#5152=CARTESIAN_POINT('Ctrl Pts',(-2.91571696477754,1.37648352458801,306.098076160255));
#5153=CARTESIAN_POINT('Ctrl Pts',(-2.95705102247069,1.28529051520153,306.104232299082));
#5154=CARTESIAN_POINT('Ctrl Pts',(-2.99405841563676,1.19236394035324,306.110388437908));
#5155=CARTESIAN_POINT('Ctrl Pts',(-3.03106246233952,1.09944576856569,306.116544020055));
#5156=CARTESIAN_POINT('Ctrl Pts',(-3.06374046223571,1.00479474580364,306.122699602201));
#5157=CARTESIAN_POINT('Ctrl Pts',(-3.09194232469225,0.908851045703676,306.128855184347));
#5158=CARTESIAN_POINT('Ctrl Pts',(-3.12014914255469,0.812890487143475,306.135011848103));
#5159=CARTESIAN_POINT('Ctrl Pts',(-3.14387813842437,0.715637215955306,306.141168511859));
#5160=CARTESIAN_POINT('Ctrl Pts',(-3.16302947394644,0.617545228664362,306.147325175615));
#5161=CARTESIAN_POINT('Ctrl Pts',(-3.18220108500312,0.519349391306045,306.153488357436));
#5162=CARTESIAN_POINT('Ctrl Pts',(-3.19678527627672,0.420313491141804,306.159651539257));
#5163=CARTESIAN_POINT('Ctrl Pts',(-3.20673363715653,0.320900206962954,306.165814721078));
#5164=CARTESIAN_POINT('Ctrl Pts',(-3.2166877094249,0.221429849272094,306.171981441203));
#5165=CARTESIAN_POINT('Ctrl Pts',(-3.22200062815385,0.121582108828924,306.178148161329));
#5166=CARTESIAN_POINT('Ctrl Pts',(-3.22267612359271,0.0218212035753486,
306.184314881454));
#5167=CARTESIAN_POINT('Ctrl Pts',(-3.22335269893809,-0.078099188251534,
306.190491460241));
#5168=CARTESIAN_POINT('Ctrl Pts',(-3.21937706276582,-0.17793203468609,306.196668039028));
#5169=CARTESIAN_POINT('Ctrl Pts',(-3.21080495877509,-0.27721666473225,306.202844617815));
#5170=CARTESIAN_POINT('Ctrl Pts',(-3.20548941632324,-0.338782841063894,
306.206674700463));
#5171=CARTESIAN_POINT('Ctrl Pts',(-3.19840746086269,-0.400138356556447,
306.210504783111));
#5172=CARTESIAN_POINT('Ctrl Pts',(-3.18958220591318,-0.461175578518668,
306.214334865759));
#5173=CARTESIAN_POINT('Ctrl Pts',(-3.17531600614771,-0.559843459120906,
306.220526270368));
#5174=CARTESIAN_POINT('Ctrl Pts',(-3.15644338444273,-0.658013392929032,
306.226717674978));
#5175=CARTESIAN_POINT('Ctrl Pts',(-3.13301053890264,-0.755223493824845,
306.232909079587));
#5176=CARTESIAN_POINT('Ctrl Pts',(-3.109608797346,-0.852304561250731,306.239092265931));
#5177=CARTESIAN_POINT('Ctrl Pts',(-3.08165896594509,-0.94842791267856,306.245275452275));
#5178=CARTESIAN_POINT('Ctrl Pts',(-3.0492587632197,-1.04313880065305,306.251458638618));
#5179=CARTESIAN_POINT('Ctrl Pts',(-3.01603218714236,-1.14026530789463,306.25779952831));
#5180=CARTESIAN_POINT('Ctrl Pts',(-2.97812518973203,-1.23590586522933,306.264140418001));
#5181=CARTESIAN_POINT('Ctrl Pts',(-2.93569870836832,-1.32958288804595,306.270481307692));
#5182=CARTESIAN_POINT('Ctrl Pts',(-2.89440134291617,-1.42076684017628,306.276653444302));
#5183=CARTESIAN_POINT('Ctrl Pts',(-2.84882222087939,-1.51009003848377,306.282825580912));
#5184=CARTESIAN_POINT('Ctrl Pts',(-2.79915925542181,-1.59713024681346,306.288997717523));
#5185=CARTESIAN_POINT('Ctrl Pts',(-2.74951451705358,-1.68413851001784,306.295167588862));
#5186=CARTESIAN_POINT('Ctrl Pts',(-2.69578912819948,-1.76886507464778,306.301337460201));
#5187=CARTESIAN_POINT('Ctrl Pts',(-2.63822703105574,-1.85091212517148,306.30750733154));
#5188=CARTESIAN_POINT('Ctrl Pts',(-2.58067093502755,-1.9329506219097,306.313676559641));
#5189=CARTESIAN_POINT('Ctrl Pts',(-2.51927917443115,-2.01230980750277,306.319845787742));
#5190=CARTESIAN_POINT('Ctrl Pts',(-2.45433856368175,-2.08862150169067,306.326015015844));
#5191=CARTESIAN_POINT('Ctrl Pts',(-2.38624504605583,-2.16863817589936,306.332483763791));
#5192=CARTESIAN_POINT('Ctrl Pts',(-2.3142497026075,-2.2453035666458,306.338952511738));
#5193=CARTESIAN_POINT('Ctrl Pts',(-2.23872910567104,-2.31823414562061,306.345421259684));
#5194=CARTESIAN_POINT('Ctrl Pts',(-2.16662622299446,-2.38786422261512,306.351597261904));
#5195=CARTESIAN_POINT('Ctrl Pts',(-2.09131057325942,-2.4540898996024,306.357773264123));
#5196=CARTESIAN_POINT('Ctrl Pts',(-2.01314499640124,-2.51661772742001,306.363949266342));
#5197=CARTESIAN_POINT('Ctrl Pts',(-1.93493489802835,-2.57918116981014,306.370128786286));
#5198=CARTESIAN_POINT('Ctrl Pts',(-1.85387198813786,-2.63804231506044,306.37630830623));
#5199=CARTESIAN_POINT('Ctrl Pts',(-1.77034878227916,-2.6929505661231,306.382487826174));
#5200=CARTESIAN_POINT('Ctrl Pts',(-1.6867174754312,-2.74792988289973,306.388675344041));
#5201=CARTESIAN_POINT('Ctrl Pts',(-1.60061988868109,-2.79894587746375,306.394862861909));
#5202=CARTESIAN_POINT('Ctrl Pts',(-1.51247353856827,-2.8457936252706,306.401050379776));
#5203=CARTESIAN_POINT('Ctrl Pts',(-1.50017648070243,-2.85232922731116,306.401913583586));
#5204=CARTESIAN_POINT('Ctrl Pts',(-1.4878395809603,-2.85878378235245,306.402776787397));
#5205=CARTESIAN_POINT('Ctrl Pts',(-1.47546400239267,-2.86515680899727,306.403639991207));
#5206=CARTESIAN_POINT('Ctrl Pts',(3.22274915228586,0.0023375073901473,305.562210368046));
#5207=CARTESIAN_POINT('Ctrl Pts',(3.22279738454772,-0.0641608838811988,
305.558419269476));
#5208=CARTESIAN_POINT('Ctrl Pts',(3.22078741422796,-0.130642986175323,305.554593488903));
#5209=CARTESIAN_POINT('Ctrl Pts',(3.21376905799516,-0.24523453273071,305.547898612221));
#5210=CARTESIAN_POINT('Ctrl Pts',(3.20973188335,-0.293381060341542,305.545055013601));
#5211=CARTESIAN_POINT('Ctrl Pts',(3.20079801594267,-0.377236269941363,305.540036903916));
#5212=CARTESIAN_POINT('Ctrl Pts',(3.19638170288744,-0.412987894215753,305.537876554609));
#5213=CARTESIAN_POINT('Ctrl Pts',(3.18678008582499,-0.481285696811891,305.533705256271));
#5214=CARTESIAN_POINT('Ctrl Pts',(3.18169300051384,-0.513841187180296,305.531697528279));
#5215=CARTESIAN_POINT('Ctrl Pts',(3.16990460305418,-0.582375680949159,305.527427145115));
#5216=CARTESIAN_POINT('Ctrl Pts',(3.16308784364899,-0.61832980479687,305.525161172483));
#5217=CARTESIAN_POINT('Ctrl Pts',(3.14447933456213,-0.708097190678513,305.519436008275));
#5218=CARTESIAN_POINT('Ctrl Pts',(3.13191760949911,-0.761737107938731,305.515953416078));
#5219=CARTESIAN_POINT('Ctrl Pts',(3.05734023786875,-1.04704244149266,305.497088532235));
#5220=CARTESIAN_POINT('Ctrl Pts',(2.97099276275974,-1.27153250959755,305.48094824535));
#5221=CARTESIAN_POINT('Ctrl Pts',(2.81407054632813,-1.57395003949105,305.457983127357));
#5222=CARTESIAN_POINT('Ctrl Pts',(2.76337950172971,-1.6613390229864,305.451198597535));
#5223=CARTESIAN_POINT('Ctrl Pts',(2.68515676415591,-1.78267591450199,305.441682256568));
#5224=CARTESIAN_POINT('Ctrl Pts',(2.66091118365575,-1.81866771901611,305.438846968483));
#5225=CARTESIAN_POINT('Ctrl Pts',(2.61605893058713,-1.88243139100973,305.433815529988));
#5226=CARTESIAN_POINT('Ctrl Pts',(2.59571828446063,-1.91038191911443,305.431607030086));
#5227=CARTESIAN_POINT('Ctrl Pts',(2.56226331397612,-1.95483196796648,305.428096855314));
#5228=CARTESIAN_POINT('Ctrl Pts',(2.54943041332456,-1.97153898075036,305.426778000909));
#5229=CARTESIAN_POINT('Ctrl Pts',(2.52313439430977,-2.00508732356597,305.424132674688));
#5230=CARTESIAN_POINT('Ctrl Pts',(2.50966434298004,-2.02192168314089,305.422806735148));
#5231=CARTESIAN_POINT('Ctrl Pts',(2.47266357033739,-2.06722432989454,305.41923866428));
#5232=CARTESIAN_POINT('Ctrl Pts',(2.44881012460269,-2.09542615990716,305.417017615641));
#5233=CARTESIAN_POINT('Ctrl Pts',(2.30227811936734,-2.26274961630145,305.403797837255));
#5234=CARTESIAN_POINT('Ctrl Pts',(2.16824835500139,-2.39149207429904,305.393433162139));
#5235=CARTESIAN_POINT('Ctrl Pts',(1.86767476857334,-2.63404527363734,305.371755889497));
#5236=CARTESIAN_POINT('Ctrl Pts',(1.700058864202,-2.74521274179289,305.360468491671));
#5237=CARTESIAN_POINT('Ctrl Pts',(1.47732750217437,-2.86466940300555,305.345533701254));
#5238=CARTESIAN_POINT('Ctrl Pts',(1.43086597756843,-2.88815675575768,305.342423901105));
#5239=CARTESIAN_POINT('Ctrl Pts',(1.35127887614507,-2.92599800070194,305.337094330183));
#5240=CARTESIAN_POINT('Ctrl Pts',(1.31844317752434,-2.94093970158709,305.334894801031));
#5241=CARTESIAN_POINT('Ctrl Pts',(1.25524343168215,-2.96842726017984,305.330656773708));
#5242=CARTESIAN_POINT('Ctrl Pts',(1.22492468307446,-2.98106623007257,305.328621721622));
#5243=CARTESIAN_POINT('Ctrl Pts',(1.14387956744896,-3.01340638411414,305.323174289503));
#5244=CARTESIAN_POINT('Ctrl Pts',(1.09284015930307,-3.0322892878481,305.319735805423));
#5245=CARTESIAN_POINT('Ctrl Pts',(0.815397097240796,-3.12701961240845,305.300992656832));
#5246=CARTESIAN_POINT('Ctrl Pts',(0.581602149451182,-3.17880935548137,305.284935039072));
#5247=CARTESIAN_POINT('Ctrl Pts',(0.242410204319315,-3.215253009967,305.261939713227));
#5248=CARTESIAN_POINT('Ctrl Pts',(0.140072620152158,-3.22133453201706,305.2550527869));
#5249=CARTESIAN_POINT('Ctrl Pts',(-0.00614124198249999,-3.22304122512347,
305.24541150769));
#5250=CARTESIAN_POINT('Ctrl Pts',(-0.0499056063542504,-3.22266073704752,
305.242551356178));
#5251=CARTESIAN_POINT('Ctrl Pts',(-0.128422588832258,-3.22037813324722,
305.2374807151));
#5252=CARTESIAN_POINT('Ctrl Pts',(-0.163177660860009,-3.21880427427332,
305.235257624708));
#5253=CARTESIAN_POINT('Ctrl Pts',(-0.218982064994394,-3.21537096920916,
305.231729555455));
#5254=CARTESIAN_POINT('Ctrl Pts',(-0.240049704208506,-3.21386680230251,
305.230407131546));
#5255=CARTESIAN_POINT('Ctrl Pts',(-0.282547455671316,-3.21041234903641,
305.227760779551));
#5256=CARTESIAN_POINT('Ctrl Pts',(-0.303975766826593,-3.20845434886205,
305.226437294569));
#5257=CARTESIAN_POINT('Ctrl Pts',(-0.361919166548094,-3.2025740706638,305.222884104706));
#5258=CARTESIAN_POINT('Ctrl Pts',(-0.398390459072767,-3.19824193193941,
305.220675181146));
#5259=CARTESIAN_POINT('Ctrl Pts',(-0.62256497884837,-3.16771949301166,305.207224627413));
#5260=CARTESIAN_POINT('Ctrl Pts',(-0.807748577709249,-3.12563464350403,
305.196647578715));
#5261=CARTESIAN_POINT('Ctrl Pts',(-1.1559066838095,-3.01347817234163,305.176117070411));
#5262=CARTESIAN_POINT('Ctrl Pts',(-1.31887666628459,-2.94579427557508,305.166204995306));
#5263=CARTESIAN_POINT('Ctrl Pts',(-1.47546404664855,-2.86515678620691,305.155887179421));
#5264=CARTESIAN_POINT('',(3.22274911409335,-0.00238958375982015,305.314226550667));
#5265=CARTESIAN_POINT('Ctrl Pts',(-1.47546400239266,-2.86515680899727,304.907226776837));
#5266=CARTESIAN_POINT('Ctrl Pts',(-1.38661581666349,-2.91091077935925,304.913390624609));
#5267=CARTESIAN_POINT('Ctrl Pts',(-1.29556523018675,-2.95256529986578,304.919554472382));
#5268=CARTESIAN_POINT('Ctrl Pts',(-1.20272725222983,-2.98991048682794,304.925718320154));
#5269=CARTESIAN_POINT('Ctrl Pts',(-1.10992910335228,-3.02723965206657,304.931879523531));
#5270=CARTESIAN_POINT('Ctrl Pts',(-1.01534548768882,-3.06026299628952,304.938040726907));
#5271=CARTESIAN_POINT('Ctrl Pts',(-0.919412680228528,-3.0888182021503,304.944201930284));
#5272=CARTESIAN_POINT('Ctrl Pts',(-0.823495604790409,-3.11736872524254,
304.950362123285));
#5273=CARTESIAN_POINT('Ctrl Pts',(-0.726230192106002,-3.14145244322592,
304.956522316285));
#5274=CARTESIAN_POINT('Ctrl Pts',(-0.628068269559386,-3.16095678731499,
304.962682509286));
#5275=CARTESIAN_POINT('Ctrl Pts',(-0.529896429498429,-3.18046310197072,
304.968843324665));
#5276=CARTESIAN_POINT('Ctrl Pts',(-0.430828324213773,-3.19538903968609,
304.975004140043));
#5277=CARTESIAN_POINT('Ctrl Pts',(-0.331325398497885,-3.20567325889745,
304.981164955422));
#5278=CARTESIAN_POINT('Ctrl Pts',(-0.231722120686853,-3.21596785009474,
304.987331984193));
#5279=CARTESIAN_POINT('Ctrl Pts',(-0.131683577892903,-3.22161132786834,
304.993499012964));
#5280=CARTESIAN_POINT('Ctrl Pts',(-0.0316756594900992,-3.2225943298988,
304.999666041735));
#5281=CARTESIAN_POINT('Ctrl Pts',(0.068382807393181,-3.2235778287825,305.005836187598));
#5282=CARTESIAN_POINT('Ctrl Pts',(0.168410186318461,-3.21989617493667,305.012006333462));
#5283=CARTESIAN_POINT('Ctrl Pts',(0.267943338381552,-3.21159211761347,305.018176479325));
#5284=CARTESIAN_POINT('Ctrl Pts',(0.367642069890415,-3.20327424598637,305.024356889601));
#5285=CARTESIAN_POINT('Ctrl Pts',(0.466844502000891,-3.19031866253762,305.030537299877));
#5286=CARTESIAN_POINT('Ctrl Pts',(0.565095113419139,-3.17281973570668,305.036717710153));
#5287=CARTESIAN_POINT('Ctrl Pts',(0.651733872217161,-3.15738893808573,305.042167682092));
#5288=CARTESIAN_POINT('Ctrl Pts',(0.737632465830545,-3.13842606930804,305.047617654031));
#5289=CARTESIAN_POINT('Ctrl Pts',(0.822488845369692,-3.11602786600865,305.053067625969));
#5290=CARTESIAN_POINT('Ctrl Pts',(0.918739972166001,-3.09062197057113,305.059249435079));
#5291=CARTESIAN_POINT('Ctrl Pts',(1.01397585255009,-3.06070922671192,305.06543124419));
#5292=CARTESIAN_POINT('Ctrl Pts',(1.10774393125943,-3.02638744136601,305.0716130533));
#5293=CARTESIAN_POINT('Ctrl Pts',(1.20138812469359,-2.99211100155645,305.077786695077));
#5294=CARTESIAN_POINT('Ctrl Pts',(1.29356796830591,-2.95343724725102,305.083960336855));
#5295=CARTESIAN_POINT('Ctrl Pts',(1.38384380190918,-2.91051436938861,305.090133978632));
#5296=CARTESIAN_POINT('Ctrl Pts',(1.47402678665652,-2.86763563778266,305.096301270808));
#5297=CARTESIAN_POINT('Ctrl Pts',(1.56230926626287,-2.82051665690766,305.102468562983));
#5298=CARTESIAN_POINT('Ctrl Pts',(1.64827027679501,-2.76935419495848,305.108635855159));
#5299=CARTESIAN_POINT('Ctrl Pts',(1.73417117034408,-2.71822751356654,305.114798834228));
#5300=CARTESIAN_POINT('Ctrl Pts',(1.81775345210234,-2.66306319446985,305.120961813297));
#5301=CARTESIAN_POINT('Ctrl Pts',(1.89862035653628,-2.60410412699762,305.127124792366));
#5302=CARTESIAN_POINT('Ctrl Pts',(1.97945835455678,-2.54516613483665,305.133285568438));
#5303=CARTESIAN_POINT('Ctrl Pts',(2.05758255485718,-2.48243634467617,305.139446344509));
#5304=CARTESIAN_POINT('Ctrl Pts',(2.13262555474417,-2.41620069649691,305.14560712058));
#5305=CARTESIAN_POINT('Ctrl Pts',(2.20766161821294,-2.3499711706496,305.151767327195));
#5306=CARTESIAN_POINT('Ctrl Pts',(2.27961672326234,-2.28023671765377,305.15792753381));
#5307=CARTESIAN_POINT('Ctrl Pts',(2.34815768035134,-2.2073226023187,305.164087740424));
#5308=CARTESIAN_POINT('Ctrl Pts',(2.41671046669684,-2.13439590297826,305.170249010209));
#5309=CARTESIAN_POINT('Ctrl Pts',(2.48184763821471,-2.05828876652911,305.176410279993));
#5310=CARTESIAN_POINT('Ctrl Pts',(2.54327458513247,-1.97936149985779,305.182571549778));
#5311=CARTESIAN_POINT('Ctrl Pts',(2.60476595634082,-1.90035145464352,305.188739281472));
#5312=CARTESIAN_POINT('Ctrl Pts',(2.66253906736249,-1.81851571582787,305.194907013167));
#5313=CARTESIAN_POINT('Ctrl Pts',(2.71634125793352,-1.73424558034557,305.201074744862));
#5314=CARTESIAN_POINT('Ctrl Pts',(2.77017409543476,-1.64992744271069,305.207245989835));
#5315=CARTESIAN_POINT('Ctrl Pts',(2.82003129213083,-1.56317252181083,305.213417234808));
#5316=CARTESIAN_POINT('Ctrl Pts',(2.8657059933397,-1.47439707075025,305.219588479781));
#5317=CARTESIAN_POINT('Ctrl Pts',(2.91145303664756,-1.38548101225713,305.22576949911));
#5318=CARTESIAN_POINT('Ctrl Pts',(2.95300417532736,-1.29453842608024,305.231950518439));
#5319=CARTESIAN_POINT('Ctrl Pts',(2.99020054766132,-1.20200592646873,305.238131537769));
#5320=CARTESIAN_POINT('Ctrl Pts',(3.01297279197949,-1.14535597497329,305.241915661689));
#5321=CARTESIAN_POINT('Ctrl Pts',(3.03411379820523,-1.0881104430503,305.245699785609));
#5322=CARTESIAN_POINT('Ctrl Pts',(3.05359645756159,-1.03037189250643,305.24948390953));
#5323=CARTESIAN_POINT('Ctrl Pts',(3.09095665410658,-0.919651710159401,305.256740393916));
#5324=CARTESIAN_POINT('Ctrl Pts',(3.12231949147421,-0.806813452707642,305.263996878302));
#5325=CARTESIAN_POINT('Ctrl Pts',(3.14747759241214,-0.692461094765246,305.271253362688));
#5326=CARTESIAN_POINT('Ctrl Pts',(3.17240408855982,-0.579161461507495,305.278443044077));
#5327=CARTESIAN_POINT('Ctrl Pts',(3.19123950516091,-0.464375585045444,305.285632725466));
#5328=CARTESIAN_POINT('Ctrl Pts',(3.2038286399983,-0.348711353452439,305.292822406854));
#5329=CARTESIAN_POINT('Ctrl Pts',(3.21632152797467,-0.233931401785546,305.299957121459));
#5330=CARTESIAN_POINT('Ctrl Pts',(3.22266317951585,-0.11828658144667,305.307091836063));
#5331=CARTESIAN_POINT('Ctrl Pts',(3.22274911409335,-0.00238958375982015,
305.314226550667));
#5332=CARTESIAN_POINT('Ctrl Pts',(-1.47546400238914,-2.86515680899909,306.154894777109));
#5333=CARTESIAN_POINT('Ctrl Pts',(-1.54120577339087,-2.83130190225831,306.15009572013));
#5334=CARTESIAN_POINT('Ctrl Pts',(-1.60576667935371,-2.79519238498628,306.145364940917));
#5335=CARTESIAN_POINT('Ctrl Pts',(-1.70378779340339,-2.7358500295457,306.13815242811));
#5336=CARTESIAN_POINT('Ctrl Pts',(-1.73814339871503,-2.7141529048128,306.135618390634));
#5337=CARTESIAN_POINT('Ctrl Pts',(-1.8013865847504,-2.67251846954085,306.13093951029));
#5338=CARTESIAN_POINT('Ctrl Pts',(-1.83037619021467,-2.65274796191372,306.12878905642));
#5339=CARTESIAN_POINT('Ctrl Pts',(-1.8952869281816,-2.60690895150876,306.123957630973));
#5340=CARTESIAN_POINT('Ctrl Pts',(-1.93100442929171,-2.58056369834513,306.121287479076));
#5341=CARTESIAN_POINT('Ctrl Pts',(-2.04565014840141,-2.49228730828378,306.112665485442));
#5342=CARTESIAN_POINT('Ctrl Pts',(-2.122235963126,-2.42740554134186,306.106826040344));
#5343=CARTESIAN_POINT('Ctrl Pts',(-2.31623079573151,-2.24684584400522,306.091637293359));
#5344=CARTESIAN_POINT('Ctrl Pts',(-2.42800778127637,-2.12556377185198,306.082471941505));
#5345=CARTESIAN_POINT('Ctrl Pts',(-2.61522231912282,-1.88829198837817,306.065460915656));
#5346=CARTESIAN_POINT('Ctrl Pts',(-2.69341070268958,-1.77498344110131,306.057659415432));
#5347=CARTESIAN_POINT('Ctrl Pts',(-2.78392762681998,-1.62399175666936,306.047214502878));
#5348=CARTESIAN_POINT('Ctrl Pts',(-2.80314423472668,-1.59059245870692,306.044900923218));
#5349=CARTESIAN_POINT('Ctrl Pts',(-2.83233754541609,-1.53768050607672,306.04121806514));
#5350=CARTESIAN_POINT('Ctrl Pts',(-2.84272246467814,-1.51839594174772,306.039872192632));
#5351=CARTESIAN_POINT('Ctrl Pts',(-2.86260852849442,-1.48054880777078,306.037220927243));
#5352=CARTESIAN_POINT('Ctrl Pts',(-2.87212753092623,-1.46199716964992,306.035916614605));
#5353=CARTESIAN_POINT('Ctrl Pts',(-2.89642247136811,-1.41349557703836,306.032496764883));
#5354=CARTESIAN_POINT('Ctrl Pts',(-2.91091381170227,-1.38340646970513,306.030365569318));
#5355=CARTESIAN_POINT('Ctrl Pts',(-2.94232481132743,-1.31550669998958,306.025543578747));
#5356=CARTESIAN_POINT('Ctrl Pts',(-2.95898824271441,-1.27758422570415,306.022841835903));
#5357=CARTESIAN_POINT('Ctrl Pts',(-3.01073482689689,-1.15337286075936,306.013987431154));
#5358=CARTESIAN_POINT('Ctrl Pts',(-3.04280824483958,-1.06588436263582,306.007744111887));
#5359=CARTESIAN_POINT('Ctrl Pts',(-3.14979881620179,-0.729622568371299,
305.983981210183));
#5360=CARTESIAN_POINT('Ctrl Pts',(-3.19835445754483,-0.473449805534653,
305.966451779303));
#5361=CARTESIAN_POINT('Ctrl Pts',(-3.21904268845474,-0.162873764190184,
305.946605969192));
#5362=CARTESIAN_POINT('Ctrl Pts',(-3.22123245658054,-0.111470311267066,
305.943362372282));
#5363=CARTESIAN_POINT('Ctrl Pts',(-3.22285439103549,-0.0244166800758755,
305.937935643973));
#5364=CARTESIAN_POINT('Ctrl Pts',(-3.22292740963356,0.0112103012952112,
305.935733497365));
#5365=CARTESIAN_POINT('Ctrl Pts',(-3.22186683887805,0.0841854093056658,
305.931258748623));
#5366=CARTESIAN_POINT('Ctrl Pts',(-3.22067452399695,0.121527354379492,305.928988275965));
#5367=CARTESIAN_POINT('Ctrl Pts',(-3.21592207828865,0.217833069758899,305.923177320646));
#5368=CARTESIAN_POINT('Ctrl Pts',(-3.21138970784864,0.27673604173398,305.919666645779));
#5369=CARTESIAN_POINT('Ctrl Pts',(-3.1977306672811,0.407235606546508,305.91196103802));
#5370=CARTESIAN_POINT('Ctrl Pts',(-3.18781314804363,0.478717546992175,305.90778911631));
#5371=CARTESIAN_POINT('Ctrl Pts',(-3.14506201187071,0.72563285301452,305.893453819092));
#5372=CARTESIAN_POINT('Ctrl Pts',(-3.10007053350801,0.89862195044624,305.883560934002));
#5373=CARTESIAN_POINT('Ctrl Pts',(-2.9979694329104,1.18961433340329,305.86614767089));
#5374=CARTESIAN_POINT('Ctrl Pts',(-2.94757466662236,1.30950366840756,305.858722798735));
#5375=CARTESIAN_POINT('Ctrl Pts',(-2.87581245723878,1.45494369530914,305.849026643093));
#5376=CARTESIAN_POINT('Ctrl Pts',(-2.86110370898222,1.48365893473528,305.847077081509));
#5377=CARTESIAN_POINT('Ctrl Pts',(-2.83723961823572,1.5285728235668,305.843964348531));
#5378=CARTESIAN_POINT('Ctrl Pts',(-2.82837039630401,1.54492213356405,305.8428177914));
#5379=CARTESIAN_POINT('Ctrl Pts',(-2.80893920972284,1.58001292826479,305.840325752334));
#5380=CARTESIAN_POINT('Ctrl Pts',(-2.79833024049248,1.5987270379951,305.838977378938));
#5381=CARTESIAN_POINT('Ctrl Pts',(-2.7691493039314,1.64902149702494,305.835303875091));
#5382=CARTESIAN_POINT('Ctrl Pts',(-2.75022537698769,1.68039277687754,305.832958859233));
#5383=CARTESIAN_POINT('Ctrl Pts',(-2.70585547743292,1.75118962371925,305.827554762237));
#5384=CARTESIAN_POINT('Ctrl Pts',(-2.6800750937533,1.79039550089485,305.824480701171));
#5385=CARTESIAN_POINT('Ctrl Pts',(-2.58761037021346,1.924538424704,305.813710933626));
#5386=CARTESIAN_POINT('Ctrl Pts',(-2.51666458427771,2.01642576769474,305.805886723518));
#5387=CARTESIAN_POINT('Ctrl Pts',(-2.30197280152104,2.26546343879954,305.78371283706));
#5388=CARTESIAN_POINT('Ctrl Pts',(-2.1473806643742,2.41250575573752,305.769457067012));
#5389=CARTESIAN_POINT('Ctrl Pts',(-1.93424294673985,2.57839022501302,305.752148225552));
#5390=CARTESIAN_POINT('Ctrl Pts',(-1.88815583062837,2.61232849006755,305.748524920742));
#5391=CARTESIAN_POINT('Ctrl Pts',(-1.8107974012959,2.66617729254169,305.742632743126));
#5392=CARTESIAN_POINT('Ctrl Pts',(-1.78004455512285,2.68680668153204,305.740337609816));
#5393=CARTESIAN_POINT('Ctrl Pts',(-1.71844550132972,2.72660611407057,305.735830293627));
#5394=CARTESIAN_POINT('Ctrl Pts',(-1.68761732113617,2.74579383478301,305.733617695064));
#5395=CARTESIAN_POINT('Ctrl Pts',(-1.61078391801753,2.79183262629923,305.728204213755));
#5396=CARTESIAN_POINT('Ctrl Pts',(-1.56442399183894,2.81807244273501,305.725025114396));
#5397=CARTESIAN_POINT('Ctrl Pts',(-1.46220591709482,2.87262776001456,305.718186161945));
#5398=CARTESIAN_POINT('Ctrl Pts',(-1.40612978071229,2.90048893601899,305.714541314258));
#5399=CARTESIAN_POINT('Ctrl Pts',(-1.2278848961713,2.9826638765305,305.7032337901));
#5400=CARTESIAN_POINT('Ctrl Pts',(-1.10312596642887,3.0310230538844,305.695723447262));
#5401=CARTESIAN_POINT('Ctrl Pts',(-0.79728409916959,3.12817972548102,305.677711786067));
#5402=CARTESIAN_POINT('Ctrl Pts',(-0.614266223535925,3.1692005441263,305.66725728637));
#5403=CARTESIAN_POINT('Ctrl Pts',(-0.392195285316613,3.19900930278619,305.653938465533));
#5404=CARTESIAN_POINT('Ctrl Pts',(-0.355563765608199,3.2032876572366,305.65172063925));
#5405=CARTESIAN_POINT('Ctrl Pts',(-0.297409615858438,3.20906997831661,305.648155534628));
#5406=CARTESIAN_POINT('Ctrl Pts',(-0.275930400798075,3.21098815925837,305.64682923957));
#5407=CARTESIAN_POINT('Ctrl Pts',(-0.233376210144597,3.21435830760118,305.644179945453));
#5408=CARTESIAN_POINT('Ctrl Pts',(-0.212303112336628,3.21581888529505,305.642857431246));
#5409=CARTESIAN_POINT('Ctrl Pts',(-0.156536700056764,3.21913355842895,305.639332343744));
#5410=CARTESIAN_POINT('Ctrl Pts',(-0.121825882328664,3.2206339186488,305.637112393289));
#5411=CARTESIAN_POINT('Ctrl Pts',(-0.0434422639353102,3.22275311761159,
305.632050916455));
#5412=CARTESIAN_POINT('Ctrl Pts',(0.000232304049122911,3.22304584098117,
305.629196859065));
#5413=CARTESIAN_POINT('Ctrl Pts',(0.145939241060622,3.22106097320073,305.619589374183));
#5414=CARTESIAN_POINT('Ctrl Pts',(0.247853123107453,3.21482488036991,305.612730821619));
#5415=CARTESIAN_POINT('Ctrl Pts',(0.587494445676255,3.17779508729527,305.589701226514));
#5416=CARTESIAN_POINT('Ctrl Pts',(0.822094956060486,3.12533609918711,305.573578857673));
#5417=CARTESIAN_POINT('Ctrl Pts',(1.10009290415081,3.02966391329495,305.554784270479));
#5418=CARTESIAN_POINT('Ctrl Pts',(1.15100003995775,3.01069216165385,305.551351922311));
#5419=CARTESIAN_POINT('Ctrl Pts',(1.23188900686097,2.97819513156612,305.545910211351));
#5420=CARTESIAN_POINT('Ctrl Pts',(1.26218401024456,2.96548283012213,305.543874887003));
#5421=CARTESIAN_POINT('Ctrl Pts',(1.32537656401891,2.93782228223062,305.539633278719));
#5422=CARTESIAN_POINT('Ctrl Pts',(1.35822790940455,2.92277948291799,305.537430493718));
#5423=CARTESIAN_POINT('Ctrl Pts',(1.43794330569549,2.88464302977454,305.532086715117));
#5424=CARTESIAN_POINT('Ctrl Pts',(1.48451289960264,2.86095582990454,305.528966181846));
#5425=CARTESIAN_POINT('Ctrl Pts',(1.58414514037029,2.80719062900998,305.522277421181));
#5426=CARTESIAN_POINT('Ctrl Pts',(1.63697163585747,2.77671739887506,305.518722995895));
#5427=CARTESIAN_POINT('Ctrl Pts',(1.79728754809476,2.67807200151811,305.507864346878));
#5428=CARTESIAN_POINT('Ctrl Pts',(1.90162988284369,2.60501793374903,305.500698250105));
#5429=CARTESIAN_POINT('Ctrl Pts',(2.15794215086522,2.40193704988895,305.482338349691));
#5430=CARTESIAN_POINT('Ctrl Pts',(2.30261310545755,2.26361892423968,305.471225653588));
#5431=CARTESIAN_POINT('Ctrl Pts',(2.45696749190021,2.08583453884996,305.457211670341));
#5432=CARTESIAN_POINT('Ctrl Pts',(2.47994749324397,2.05845941820207,305.455059906568));
#5433=CARTESIAN_POINT('Ctrl Pts',(2.5159050079647,2.01414855464152,305.451576199186));
#5434=CARTESIAN_POINT('Ctrl Pts',(2.52917844559253,1.99745556677226,305.450263635706));
#5435=CARTESIAN_POINT('Ctrl Pts',(2.55539839805466,1.96380036679041,305.447614244218));
#5436=CARTESIAN_POINT('Ctrl Pts',(2.56834408048018,1.94683884243167,305.44627747202));
#5437=CARTESIAN_POINT('Ctrl Pts',(2.60255309698528,1.90108289034236,305.442670059651));
#5438=CARTESIAN_POINT('Ctrl Pts',(2.62350615554648,1.87206142787561,305.440380663702));
#5439=CARTESIAN_POINT('Ctrl Pts',(2.73341057930168,1.71436657637412,305.427959100111));
#5440=CARTESIAN_POINT('Ctrl Pts',(2.81338168121197,1.57970313136928,305.417426739239));
#5441=CARTESIAN_POINT('Ctrl Pts',(2.98280767114599,1.2404162234776,305.391852585261));
#5442=CARTESIAN_POINT('Ctrl Pts',(3.0614300791327,1.03123601340176,305.376899055731));
#5443=CARTESIAN_POINT('Ctrl Pts',(3.13208222382635,0.761147541781223,305.35902161058));
#5444=CARTESIAN_POINT('Ctrl Pts',(3.14489648417329,0.706336577932702,305.35546044052));
#5445=CARTESIAN_POINT('Ctrl Pts',(3.16371501180644,0.615128125025562,305.349641203021));
#5446=CARTESIAN_POINT('Ctrl Pts',(3.17054145761828,0.578914784215165,305.347358166146));
#5447=CARTESIAN_POINT('Ctrl Pts',(3.18231225242936,0.509999502206581,305.343062923321));
#5448=CARTESIAN_POINT('Ctrl Pts',(3.18737719530871,0.477323268478193,305.341047245641));
#5449=CARTESIAN_POINT('Ctrl Pts',(3.19688425795968,0.409064745182176,305.336877370407));
#5450=CARTESIAN_POINT('Ctrl Pts',(3.20123723659135,0.373474535477898,305.334726120791));
#5451=CARTESIAN_POINT('Ctrl Pts',(3.21002020796147,0.290147473544569,305.329737832409));
#5452=CARTESIAN_POINT('Ctrl Pts',(3.21398082970572,0.242369215415285,305.326914654041));
#5453=CARTESIAN_POINT('Ctrl Pts',(3.22083683804161,0.128987203713608,305.32028691449));
#5454=CARTESIAN_POINT('Ctrl Pts',(3.2227961534329,0.0633484734362306,305.316507037163));
#5455=CARTESIAN_POINT('Ctrl Pts',(3.22274917497873,-0.00230600822049255,
305.312761555685));
#5456=CARTESIAN_POINT('Origin',(0.,0.,177.));
#5457=CARTESIAN_POINT('',(3.933,-4.81653586104654E-16,177.));
#5458=CARTESIAN_POINT('Origin',(0.,0.,177.));
#5459=CARTESIAN_POINT('',(-1.8148060950507,-3.48926465567845,297.));
#5460=CARTESIAN_POINT('',(1.74869447533119,-3.52286199445084,297.));
#5461=CARTESIAN_POINT('Origin',(0.,0.,297.));
#5462=CARTESIAN_POINT('',(3.93481960852658,-0.00239843926903071,297.220836477965));
#5463=CARTESIAN_POINT('Ctrl Pts',(1.74869447533119,-3.52286199445084,297.));
#5464=CARTESIAN_POINT('Ctrl Pts',(2.90806357314772,-2.94736901759993,297.06547209452));
#5465=CARTESIAN_POINT('Ctrl Pts',(3.85617209864057,-1.61095470252649,297.139084253842));
#5466=CARTESIAN_POINT('Ctrl Pts',(3.93703630563088,-0.162725864948754,297.212696413163));
#5467=CARTESIAN_POINT('Ctrl Pts',(3.93582492032101,-0.00239905204916439,
297.220836477965));
#5468=CARTESIAN_POINT('',(3.93299999230081,-0.000246093130879474,298.470836477922));
#5469=CARTESIAN_POINT('Ctrl Pts',(3.93299926936306,-0.00239732969518293,
297.220836477965));
#5470=CARTESIAN_POINT('Ctrl Pts',(3.93306845839146,0.111112463605089,297.22660373228));
#5471=CARTESIAN_POINT('Ctrl Pts',(3.92821947420302,0.224824526215857,297.232370986595));
#5472=CARTESIAN_POINT('Ctrl Pts',(3.91842619360132,0.338267889843326,297.238138240911));
#5473=CARTESIAN_POINT('Ctrl Pts',(3.90864407754512,0.451581925654531,297.243898920435));
#5474=CARTESIAN_POINT('Ctrl Pts',(3.89392890351192,0.564627447569545,297.249659599959));
#5475=CARTESIAN_POINT('Ctrl Pts',(3.87430656947808,0.676932497150927,297.255420279483));
#5476=CARTESIAN_POINT('Ctrl Pts',(3.85470123276484,0.78914026549506,297.261175968973));
#5477=CARTESIAN_POINT('Ctrl Pts',(3.83019726034436,0.900608416330806,297.266931658463));
#5478=CARTESIAN_POINT('Ctrl Pts',(3.80087237107529,1.01087003061545,297.272687347953));
#5479=CARTESIAN_POINT('Ctrl Pts',(3.77156117378215,1.12108016305631,297.278440350076));
#5480=CARTESIAN_POINT('Ctrl Pts',(3.73743364047043,1.23008446439066,297.284193352198));
#5481=CARTESIAN_POINT('Ctrl Pts',(3.69861844832742,1.33742684797788,297.28994635432));
#5482=CARTESIAN_POINT('Ctrl Pts',(3.65981124973277,1.4447471256193,297.295698171677));
#5483=CARTESIAN_POINT('Ctrl Pts',(3.61631845628518,1.55040576251832,297.301449989034));
#5484=CARTESIAN_POINT('Ctrl Pts',(3.56831812451651,1.65396334972906,297.30720180639));
#5485=CARTESIAN_POINT('Ctrl Pts',(3.52031515156675,1.75752663511586,297.312953940237));
#5486=CARTESIAN_POINT('Ctrl Pts',(3.46780432886449,1.85898825253657,297.318706074083));
#5487=CARTESIAN_POINT('Ctrl Pts',(3.41101082659864,1.95793108684316,297.324458207929));
#5488=CARTESIAN_POINT('Ctrl Pts',(3.3541638766531,2.05696703505725,297.330215755038));
#5489=CARTESIAN_POINT('Ctrl Pts',(3.29302641127215,2.15347909324372,297.335973302148));
#5490=CARTESIAN_POINT('Ctrl Pts',(3.22786831331998,2.24707702401694,297.341730849258));
#5491=CARTESIAN_POINT('Ctrl Pts',(3.16268027161153,2.3407179682254,297.34749104228));
#5492=CARTESIAN_POINT('Ctrl Pts',(3.09346817959316,2.43144177848841,297.353251235301));
#5493=CARTESIAN_POINT('Ctrl Pts',(3.02054257162309,2.5188909410716,297.359011428323));
#5494=CARTESIAN_POINT('Ctrl Pts',(2.94749854717352,2.60648210345782,297.364780974737));
#5495=CARTESIAN_POINT('Ctrl Pts',(2.87072925049777,2.69078767941243,297.37055052115));
#5496=CARTESIAN_POINT('Ctrl Pts',(2.79058269164137,2.77148646778432,297.376320067564));
#5497=CARTESIAN_POINT('Ctrl Pts',(2.71412260721627,2.84847338100879,297.381824234083));
#5498=CARTESIAN_POINT('Ctrl Pts',(2.63458931482961,2.92217775913654,297.387328400602));
#5499=CARTESIAN_POINT('Ctrl Pts',(2.55231123269053,2.99235632428388,297.39283256712));
#5500=CARTESIAN_POINT('Ctrl Pts',(2.46440430868021,3.06733597418787,297.398713286935));
#5501=CARTESIAN_POINT('Ctrl Pts',(2.37304650350017,3.1385615346114,297.404594006749));
#5502=CARTESIAN_POINT('Ctrl Pts',(2.27859167607231,3.2056994515603,297.410474726564));
#5503=CARTESIAN_POINT('Ctrl Pts',(2.18425831965925,3.27275102765054,297.416347883641));
#5504=CARTESIAN_POINT('Ctrl Pts',(2.08683619493552,3.33572517840853,297.422221040719));
#5505=CARTESIAN_POINT('Ctrl Pts',(1.98671351319032,3.39432738793814,297.428094197796));
#5506=CARTESIAN_POINT('Ctrl Pts',(1.88669302508281,3.45286978311935,297.433961360235));
#5507=CARTESIAN_POINT('Ctrl Pts',(1.78397781660011,3.5070489067515,297.439828522674));
#5508=CARTESIAN_POINT('Ctrl Pts',(1.67898593072027,3.55661288931525,297.445695685113));
#5509=CARTESIAN_POINT('Ctrl Pts',(1.57195010680406,3.60714176272126,297.451677067012));
#5510=CARTESIAN_POINT('Ctrl Pts',(1.46254838908129,3.65287367102504,297.45765844891));
#5511=CARTESIAN_POINT('Ctrl Pts',(1.3512514380898,3.69359019804042,297.463639830809));
#5512=CARTESIAN_POINT('Ctrl Pts',(1.24220562620391,3.73348317539526,297.469500230753));
#5513=CARTESIAN_POINT('Ctrl Pts',(1.13134093193654,3.76856160093073,297.475360630697));
#5514=CARTESIAN_POINT('Ctrl Pts',(1.01912052783599,3.79866849695302,297.481221030641));
#5515=CARTESIAN_POINT('Ctrl Pts',(0.906917788079268,3.82877065392124,297.487080508113));
#5516=CARTESIAN_POINT('Ctrl Pts',(0.793360160715912,3.85390273093425,297.492939985585));
#5517=CARTESIAN_POINT('Ctrl Pts',(0.678925050333358,3.87395789549007,297.498799463058));
#5518=CARTESIAN_POINT('Ctrl Pts',(0.564480460267666,3.89401472139445,297.504659425923));
#5519=CARTESIAN_POINT('Ctrl Pts',(0.449158648561752,3.90899372783572,297.510519388788));
#5520=CARTESIAN_POINT('Ctrl Pts',(0.333445570025453,3.91883950319867,297.516379351654));
#5521=CARTESIAN_POINT('Ctrl Pts',(0.213536475921912,3.92904230844292,297.522451809906));
#5522=CARTESIAN_POINT('Ctrl Pts',(0.0932076757285175,3.9337324905987,297.528524268158));
#5523=CARTESIAN_POINT('Ctrl Pts',(-0.0269975551490727,3.93290733834602,
297.534596726411));
#5524=CARTESIAN_POINT('Ctrl Pts',(-0.143162287133464,3.9321099222138,297.540465069079));
#5525=CARTESIAN_POINT('Ctrl Pts',(-0.259211207929003,3.92616206917407,297.546333411748));
#5526=CARTESIAN_POINT('Ctrl Pts',(-0.374658128173509,3.91511433894255,297.552201754417));
#5527=CARTESIAN_POINT('Ctrl Pts',(-0.496128345835865,3.90349020732382,297.558376270461));
#5528=CARTESIAN_POINT('Ctrl Pts',(-0.616931525781467,3.88621976691363,297.564550786505));
#5529=CARTESIAN_POINT('Ctrl Pts',(-0.736513664123003,3.86342291531229,297.570725302549));
#5530=CARTESIAN_POINT('Ctrl Pts',(-0.85609580246454,3.84062606371095,297.576899818593));
#5531=CARTESIAN_POINT('Ctrl Pts',(-0.974456405796253,3.8123029905964,297.583074334637));
#5532=CARTESIAN_POINT('Ctrl Pts',(-1.09106157979183,3.77863383104293,297.589248850681));
#5533=CARTESIAN_POINT('Ctrl Pts',(-1.20228880561966,3.74651752706804,297.595138591821));
#5534=CARTESIAN_POINT('Ctrl Pts',(-1.31227030455785,3.709435880047,297.601028332961));
#5535=CARTESIAN_POINT('Ctrl Pts',(-1.42053173693775,3.66750304490025,297.606918074101));
#5536=CARTESIAN_POINT('Ctrl Pts',(-1.52865914675956,3.6256221206299,297.612800524018));
#5537=CARTESIAN_POINT('Ctrl Pts',(-1.63507034575995,3.57890210032103,297.618682973936));
#5538=CARTESIAN_POINT('Ctrl Pts',(-1.73930492813322,3.52750724548817,297.624565423854));
#5539=CARTESIAN_POINT('Ctrl Pts',(-1.84343785049158,3.4761625160704,297.630442136616));
#5540=CARTESIAN_POINT('Ctrl Pts',(-1.94539801331448,3.42015220315325,297.636318849379));
#5541=CARTESIAN_POINT('Ctrl Pts',(-2.04474441607394,3.3596888654955,297.642195562142));
#5542=CARTESIAN_POINT('Ctrl Pts',(-2.14580137930282,3.29818446150446,297.648173460979));
#5543=CARTESIAN_POINT('Ctrl Pts',(-2.24415333475831,3.23207241709213,297.654151359817));
#5544=CARTESIAN_POINT('Ctrl Pts',(-2.33936135744235,3.16162575889454,297.660129258654));
#5545=CARTESIAN_POINT('Ctrl Pts',(-2.43285922939206,3.09244448150049,297.665999780951));
#5546=CARTESIAN_POINT('Ctrl Pts',(-2.52332483473946,3.01908327348623,297.671870303248));
#5547=CARTESIAN_POINT('Ctrl Pts',(-2.61037181737141,2.94184431523375,297.677740825546));
#5548=CARTESIAN_POINT('Ctrl Pts',(-2.69740801732825,2.86461492471775,297.68361062065));
#5549=CARTESIAN_POINT('Ctrl Pts',(-2.78102612986177,2.78350901163158,297.689480415754));
#5550=CARTESIAN_POINT('Ctrl Pts',(-2.86087395423676,2.69886813645456,297.695350210859));
#5551=CARTESIAN_POINT('Ctrl Pts',(-2.94073087962143,2.61421761395866,297.701220674999));
#5552=CARTESIAN_POINT('Ctrl Pts',(-3.01681638079674,2.52603162682772,297.707091139139));
#5553=CARTESIAN_POINT('Ctrl Pts',(-3.08881657645025,2.4346870757956,297.71296160328));
#5554=CARTESIAN_POINT('Ctrl Pts',(-3.16312456313294,2.34041469750521,297.71902023086));
#5555=CARTESIAN_POINT('Ctrl Pts',(-3.23308065213613,2.24277823071728,297.72507885844));
#5556=CARTESIAN_POINT('Ctrl Pts',(-3.29838705336314,2.14222590923703,297.73113748602));
#5557=CARTESIAN_POINT('Ctrl Pts',(-3.36175944418768,2.04465138521739,297.737016690932));
#5558=CARTESIAN_POINT('Ctrl Pts',(-3.42075350303013,1.94433166484596,297.742895895844));
#5559=CARTESIAN_POINT('Ctrl Pts',(-3.47514360823768,1.84170190370885,297.748775100755));
#5560=CARTESIAN_POINT('Ctrl Pts',(-3.53202354445589,1.73437403138183,297.75492343967));
#5561=CARTESIAN_POINT('Ctrl Pts',(-3.58386779070879,1.62452006884419,297.761071778584));
#5562=CARTESIAN_POINT('Ctrl Pts',(-3.63047482275331,1.51266042499774,297.767220117498));
#5563=CARTESIAN_POINT('Ctrl Pts',(-3.67708185479782,1.4008007811513,297.773368456412));
#5564=CARTESIAN_POINT('Ctrl Pts',(-3.71845156387867,1.28693595500757,297.779516795327));
#5565=CARTESIAN_POINT('Ctrl Pts',(-3.75444230825449,1.17160230197313,297.785665134241));
#5566=CARTESIAN_POINT('Ctrl Pts',(-3.78884670506842,1.06135215755922,297.791542475636));
#5567=CARTESIAN_POINT('Ctrl Pts',(-3.8184469033587,0.949405204907577,297.797419817031));
#5568=CARTESIAN_POINT('Ctrl Pts',(-3.8430754740714,0.836217615570792,297.803297158426));
#5569=CARTESIAN_POINT('Ctrl Pts',(-3.86767267882028,0.723174177426265,297.809167014673));
#5570=CARTESIAN_POINT('Ctrl Pts',(-3.88731076127924,0.608893644422506,297.815036870921));
#5571=CARTESIAN_POINT('Ctrl Pts',(-3.90187169702593,0.493848417986708,297.820906727169));
#5572=CARTESIAN_POINT('Ctrl Pts',(-3.9164179628193,0.378919098119767,297.826770669612));
#5573=CARTESIAN_POINT('Ctrl Pts',(-3.92589720538806,0.263227024224401,297.832634612056));
#5574=CARTESIAN_POINT('Ctrl Pts',(-3.93024234526173,0.147255246125917,297.8384985545));
#5575=CARTESIAN_POINT('Ctrl Pts',(-3.93467542384946,0.0289363838527769,
297.844481173804));
#5576=CARTESIAN_POINT('Ctrl Pts',(-3.93376423865397,-0.0896732009304856,
297.850463793109));
#5577=CARTESIAN_POINT('Ctrl Pts',(-3.92749315512083,-0.208054119110971,
297.856446412413));
#5578=CARTESIAN_POINT('Ctrl Pts',(-3.92135332922841,-0.323957251762902,
297.86230381181));
#5579=CARTESIAN_POINT('Ctrl Pts',(-3.91007581159166,-0.439640765396489,
297.868161211208));
#5580=CARTESIAN_POINT('Ctrl Pts',(-3.89369855941713,-0.554617461312753,
297.874018610605));
#5581=CARTESIAN_POINT('Ctrl Pts',(-3.87732364307123,-0.669577758515963,
297.879875174583));
#5582=CARTESIAN_POINT('Ctrl Pts',(-3.85585049677704,-0.783831030207,297.88573173856));
#5583=CARTESIAN_POINT('Ctrl Pts',(-3.82936877675414,-0.896896745239102,
297.891588302538));
#5584=CARTESIAN_POINT('Ctrl Pts',(-3.80288445395497,-1.00997357302219,297.897445442133));
#5585=CARTESIAN_POINT('Ctrl Pts',(-3.77139067295981,-1.12186221049407,297.903302581727));
#5586=CARTESIAN_POINT('Ctrl Pts',(-3.73502772160115,-1.23209452513634,297.909159721322));
#5587=CARTESIAN_POINT('Ctrl Pts',(-3.69730099994697,-1.34646103545575,297.915236529362));
#5588=CARTESIAN_POINT('Ctrl Pts',(-3.6543328677155,-1.45904409174705,297.921313337402));
#5589=CARTESIAN_POINT('Ctrl Pts',(-3.6063353876151,-1.56934192323886,297.927390145442));
#5590=CARTESIAN_POINT('Ctrl Pts',(-3.56000478352882,-1.67580928676987,297.93325591562));
#5591=CARTESIAN_POINT('Ctrl Pts',(-3.50898858329163,-1.7801471603624,297.939121685798));
#5592=CARTESIAN_POINT('Ctrl Pts',(-3.45352462110269,-1.88192898150741,297.944987455977));
#5593=CARTESIAN_POINT('Ctrl Pts',(-3.39802257169273,-1.98378069644589,297.950857254192));
#5594=CARTESIAN_POINT('Ctrl Pts',(-3.33806689116138,-2.08307251172606,297.956727052407));
#5595=CARTESIAN_POINT('Ctrl Pts',(-3.27393888723683,-2.17940660791842,297.962596850622));
#5596=CARTESIAN_POINT('Ctrl Pts',(-3.2097214767929,-2.2758750119905,297.968474832442));
#5597=CARTESIAN_POINT('Ctrl Pts',(-3.14132037904824,-2.36937713800281,297.974352814262));
#5598=CARTESIAN_POINT('Ctrl Pts',(-3.06905726829611,-2.45954802431642,297.980230796081));
#5599=CARTESIAN_POINT('Ctrl Pts',(-3.06147350420917,-2.46901114764719,297.980847669988));
#5600=CARTESIAN_POINT('Ctrl Pts',(-3.05384723796947,-2.47843761515068,297.981464543895));
#5601=CARTESIAN_POINT('Ctrl Pts',(-3.04617886433616,-2.48782702904998,297.982081417801));
#5602=CARTESIAN_POINT('Ctrl Pts',(-2.97306131840848,-2.57735460488876,297.987963278591));
#5603=CARTESIAN_POINT('Ctrl Pts',(-2.89587582608214,-2.66380025802543,297.99384513938));
#5604=CARTESIAN_POINT('Ctrl Pts',(-2.8149117811643,-2.74677277259376,297.99972700017));
#5605=CARTESIAN_POINT('Ctrl Pts',(-2.73405011246422,-2.82964037130435,298.005601423551));
#5606=CARTESIAN_POINT('Ctrl Pts',(-2.64941967868757,-2.90904327365463,298.011475846932));
#5607=CARTESIAN_POINT('Ctrl Pts',(-2.56135058815952,-2.98462261676998,298.017350270313));
#5608=CARTESIAN_POINT('Ctrl Pts',(-2.4733695321063,-3.0601264102488,298.02321882158));
#5609=CARTESIAN_POINT('Ctrl Pts',(-2.38195696772714,-3.13181398091997,298.029087372847));
#5610=CARTESIAN_POINT('Ctrl Pts',(-2.28747990829278,-3.19936316618743,298.034955924114));
#5611=CARTESIAN_POINT('Ctrl Pts',(-2.19119404201578,-3.26820561173689,298.040936831499));
#5612=CARTESIAN_POINT('Ctrl Pts',(-2.09172543363303,-3.33274926684149,298.046917738884));
#5613=CARTESIAN_POINT('Ctrl Pts',(-1.98949837687786,-3.3926958614648,298.05289864627));
#5614=CARTESIAN_POINT('Ctrl Pts',(-1.88930232427782,-3.45145146236658,298.058760727503));
#5615=CARTESIAN_POINT('Ctrl Pts',(-1.78645679038421,-3.50579076493241,298.064622808737));
#5616=CARTESIAN_POINT('Ctrl Pts',(-1.68139000228497,-3.55547699475276,298.07048488997));
#5617=CARTESIAN_POINT('Ctrl Pts',(-1.57633784817784,-3.60515630413795,298.076346154717));
#5618=CARTESIAN_POINT('Ctrl Pts',(-1.46906542726807,-3.65018365366576,298.082207419464));
#5619=CARTESIAN_POINT('Ctrl Pts',(-1.36002385382962,-3.69036910308636,298.088068684211));
#5620=CARTESIAN_POINT('Ctrl Pts',(-1.2509713171273,-3.73055859283462,298.093930538261));
#5621=CARTESIAN_POINT('Ctrl Pts',(-1.14014966065168,-3.76590507234974,298.099792392312));
#5622=CARTESIAN_POINT('Ctrl Pts',(-1.02802752287924,-3.79626769501345,298.105654246362));
#5623=CARTESIAN_POINT('Ctrl Pts',(-0.911918583241552,-3.82770994176456,
298.111724534279));
#5624=CARTESIAN_POINT('Ctrl Pts',(-0.794415415532427,-3.85380717801685,
298.117794822195));
#5625=CARTESIAN_POINT('Ctrl Pts',(-0.676051312214117,-3.87446042995067,
298.123865110112));
#5626=CARTESIAN_POINT('Ctrl Pts',(-0.561583339555891,-3.89443384935222,
298.129735585465));
#5627=CARTESIAN_POINT('Ctrl Pts',(-0.446310640159776,-3.90931604677284,
298.135606060819));
#5628=CARTESIAN_POINT('Ctrl Pts',(-0.330720874565897,-3.91907038762082,
298.141476536172));
#5629=CARTESIAN_POINT('Ctrl Pts',(-0.209229639513829,-3.92932273920792,
298.14764673037));
#5630=CARTESIAN_POINT('Ctrl Pts',(-0.0873886365315712,-3.93390978520482,
298.153816924568));
#5631=CARTESIAN_POINT('Ctrl Pts',(0.0342372277062223,-3.9328509776292,298.159987118767));
#5632=CARTESIAN_POINT('Ctrl Pts',(0.155863091944016,-3.93179217005359,298.166157312965));
#5633=CARTESIAN_POINT('Ctrl Pts',(0.2772733014266,-3.9250876078748,298.172327507163));
#5634=CARTESIAN_POINT('Ctrl Pts',(0.397912027585362,-3.91281931838194,298.178497701361));
#5635=CARTESIAN_POINT('Ctrl Pts',(0.51292160164584,-3.9011234824431,298.18437998667));
#5636=CARTESIAN_POINT('Ctrl Pts',(0.627599782461963,-3.88433385978971,298.190262271979));
#5637=CARTESIAN_POINT('Ctrl Pts',(0.741460574344983,-3.86247656519648,298.196144557288));
#5638=CARTESIAN_POINT('Ctrl Pts',(0.855177758129014,-3.84064683834166,298.202019423505));
#5639=CARTESIAN_POINT('Ctrl Pts',(0.968079202550166,-3.81376222860767,298.207894289721));
#5640=CARTESIAN_POINT('Ctrl Pts',(1.0796834978317,-3.78190065238498,298.213769155937));
#5641=CARTESIAN_POINT('Ctrl Pts',(1.19117657663295,-3.75007082702236,298.219638167701));
#5642=CARTESIAN_POINT('Ctrl Pts',(1.30137468405352,-3.71327401370545,298.225507179466));
#5643=CARTESIAN_POINT('Ctrl Pts',(1.40980672183624,-3.67163914445107,298.23137619123));
#5644=CARTESIAN_POINT('Ctrl Pts',(1.52030300364343,-3.629211663236,298.237356932634));
#5645=CARTESIAN_POINT('Ctrl Pts',(1.6289648586505,-3.58176011558691,298.243337674038));
#5646=CARTESIAN_POINT('Ctrl Pts',(1.73530974020645,-3.52947433841707,298.249318415442));
#5647=CARTESIAN_POINT('Ctrl Pts',(1.83955361368677,-3.47822154787025,298.255180998023));
#5648=CARTESIAN_POINT('Ctrl Pts',(1.94157083928183,-3.42232398115469,298.261043580604));
#5649=CARTESIAN_POINT('Ctrl Pts',(2.04092787734249,-3.36200868521875,298.266906163185));
#5650=CARTESIAN_POINT('Ctrl Pts',(2.14027132221888,-3.30170164110822,298.272767943698));
#5651=CARTESIAN_POINT('Ctrl Pts',(2.23695495152024,-3.23697828332267,298.278629724211));
#5652=CARTESIAN_POINT('Ctrl Pts',(2.33057171244451,-3.16811055570248,298.284491504723));
#5653=CARTESIAN_POINT('Ctrl Pts',(2.42419810691866,-3.09923574130976,298.290353888437));
#5654=CARTESIAN_POINT('Ctrl Pts',(2.51475667401381,-3.02621595322321,298.296216272151));
#5655=CARTESIAN_POINT('Ctrl Pts',(2.60187168643205,-2.94936480065509,298.302078655865));
#5656=CARTESIAN_POINT('Ctrl Pts',(2.69206609233749,-2.8697970676477,298.30814826662));
#5657=CARTESIAN_POINT('Ctrl Pts',(2.7785686291232,-2.78612240259129,298.314217877374));
#5658=CARTESIAN_POINT('Ctrl Pts',(2.86100312929294,-2.69873120080085,298.320287488129));
#5659=CARTESIAN_POINT('Ctrl Pts',(2.94074067128642,-2.61419912250503,298.326158523211));
#5660=CARTESIAN_POINT('Ctrl Pts',(3.01667197149979,-2.5261902455251,298.332029558292));
#5661=CARTESIAN_POINT('Ctrl Pts',(3.08849779704574,-2.43509144749096,298.337900593374));
#5662=CARTESIAN_POINT('Ctrl Pts',(3.16396766357847,-2.33937080555374,298.344069491965));
#5663=CARTESIAN_POINT('Ctrl Pts',(3.23490424229983,-2.24023891656768,298.350238390556));
#5664=CARTESIAN_POINT('Ctrl Pts',(3.30101281914729,-2.13817758098462,298.356407289148));
#5665=CARTESIAN_POINT('Ctrl Pts',(3.36712139599475,-2.03611624540157,298.362576187739));
#5666=CARTESIAN_POINT('Ctrl Pts',(3.42840176972213,-1.9311259475968,298.36874508633));
#5667=CARTESIAN_POINT('Ctrl Pts',(3.48461638307562,-1.82371534588077,298.374913984921));
#5668=CARTESIAN_POINT('Ctrl Pts',(3.54119133411491,-1.71561623835913,298.381122426373));
#5669=CARTESIAN_POINT('Ctrl Pts',(3.59280149957876,-1.60475036607249,298.387330867826));
#5670=CARTESIAN_POINT('Ctrl Pts',(3.63918375830147,-1.49158659598255,298.393539309278));
#5671=CARTESIAN_POINT('Ctrl Pts',(3.68730664204182,-1.37417603639303,298.399980739998));
#5672=CARTESIAN_POINT('Ctrl Pts',(3.72980133461905,-1.25429201603047,298.406422170718));
#5673=CARTESIAN_POINT('Ctrl Pts',(3.76642526142513,-1.13248830020386,298.412863601439));
#5674=CARTESIAN_POINT('Ctrl Pts',(3.80157304731997,-1.01559392817932,298.419045407912));
#5675=CARTESIAN_POINT('Ctrl Pts',(3.83131393489967,-0.896931964919147,298.425227214386));
#5676=CARTESIAN_POINT('Ctrl Pts',(3.85548160318599,-0.777013904312119,298.431409020859));
#5677=CARTESIAN_POINT('Ctrl Pts',(3.87961344366601,-0.657273618449312,298.437581662999));
#5678=CARTESIAN_POINT('Ctrl Pts',(3.8981884529318,-0.536281279144689,298.44375430514));
#5679=CARTESIAN_POINT('Ctrl Pts',(3.91109020884378,-0.414562876155478,298.44992694728));
#5680=CARTESIAN_POINT('Ctrl Pts',(3.92396831058168,-0.293067632580642,298.456088272453));
#5681=CARTESIAN_POINT('Ctrl Pts',(3.93119385558125,-0.170849319328,298.462249597626));
#5682=CARTESIAN_POINT('Ctrl Pts',(3.93270165298957,-0.0484428382023322,
298.468410922799));
#5683=CARTESIAN_POINT('Ctrl Pts',(3.93289951333215,-0.0323800779427963,
298.469219441173));
#5684=CARTESIAN_POINT('Ctrl Pts',(3.93299898690451,-0.0163140899041396,
298.470027959547));
#5685=CARTESIAN_POINT('Ctrl Pts',(3.93299999230081,-0.000246093130890435,
298.470836477922));
#5686=CARTESIAN_POINT('',(3.93299898658193,0.00282339255091959,299.720836477927));
#5687=CARTESIAN_POINT('Ctrl Pts',(3.93299999230086,-0.000246092268270265,
298.470836477965));
#5688=CARTESIAN_POINT('Ctrl Pts',(3.93300758397887,0.121082666815665,298.476941565764));
#5689=CARTESIAN_POINT('Ctrl Pts',(3.92739656637158,0.242318400603063,298.483046653563));
#5690=CARTESIAN_POINT('Ctrl Pts',(3.91621860102681,0.362933697762562,298.489151741363));
#5691=CARTESIAN_POINT('Ctrl Pts',(3.90502744511325,0.483691327119881,298.495264033477));
#5692=CARTESIAN_POINT('Ctrl Pts',(3.88825627369643,0.603826702702683,298.501376325591));
#5693=CARTESIAN_POINT('Ctrl Pts',(3.8660081877617,0.722820650064391,298.507488617705));
#5694=CARTESIAN_POINT('Ctrl Pts',(3.84371180437189,0.842072916494249,298.513614178742));
#5695=CARTESIAN_POINT('Ctrl Pts',(3.81591481002405,0.960178448721801,298.51973973978));
#5696=CARTESIAN_POINT('Ctrl Pts',(3.78277103273396,1.0766300729168,298.525865300818));
#5697=CARTESIAN_POINT('Ctrl Pts',(3.74958808912236,1.19321930912004,298.53199810049));
#5698=CARTESIAN_POINT('Ctrl Pts',(3.71104587195854,1.30815039850082,298.538130900162));
#5699=CARTESIAN_POINT('Ctrl Pts',(3.66734688988072,1.42093482935785,298.544263699834));
#5700=CARTESIAN_POINT('Ctrl Pts',(3.62355526516608,1.53395836525966,298.550409501154));
#5701=CARTESIAN_POINT('Ctrl Pts',(3.57458516905893,1.64482581782616,298.556555302473));
#5702=CARTESIAN_POINT('Ctrl Pts',(3.52068620194426,1.75307092481716,298.562701103792));
#5703=CARTESIAN_POINT('Ctrl Pts',(3.49546014165026,1.8037323334055,298.565577492022));
#5704=CARTESIAN_POINT('Ctrl Pts',(3.46915506050871,1.85381971458082,298.568453880252));
#5705=CARTESIAN_POINT('Ctrl Pts',(3.441799798319,1.90328745813429,298.571330268483));
#5706=CARTESIAN_POINT('Ctrl Pts',(3.38586408220222,2.00443851423291,298.577211873066));
#5707=CARTESIAN_POINT('Ctrl Pts',(3.3253754113875,2.10328456294611,298.58309347765));
#5708=CARTESIAN_POINT('Ctrl Pts',(3.26054858194923,2.19938899350453,298.588975082234));
#5709=CARTESIAN_POINT('Ctrl Pts',(3.19580367793401,2.29537197132188,298.594849253893));
#5710=CARTESIAN_POINT('Ctrl Pts',(3.1267317472171,2.38861988338595,298.600723425552));
#5711=CARTESIAN_POINT('Ctrl Pts',(3.05359342725983,2.4787206742583,298.606597597212));
#5712=CARTESIAN_POINT('Ctrl Pts',(2.98052816033606,2.56873146940617,298.612465901549));
#5713=CARTESIAN_POINT('Ctrl Pts',(2.90340484192547,2.65560107857684,298.618334205886));
#5714=CARTESIAN_POINT('Ctrl Pts',(2.82252697930556,2.73894696025538,298.624202510223));
#5715=CARTESIAN_POINT('Ctrl Pts',(2.74009590391267,2.82389345159158,298.630183511966));
#5716=CARTESIAN_POINT('Ctrl Pts',(2.65376483056407,2.90517911534441,298.636164513708));
#5717=CARTESIAN_POINT('Ctrl Pts',(2.56389795662498,2.98243462091196,298.642145515451));
#5718=CARTESIAN_POINT('Ctrl Pts',(2.47582141525793,3.05815103824905,298.648007363363));
#5719=CARTESIAN_POINT('Ctrl Pts',(2.38434897673669,3.1299961093033,298.653869211275));
#5720=CARTESIAN_POINT('Ctrl Pts',(2.28985963840239,3.19766036914737,298.659731059188));
#5721=CARTESIAN_POINT('Ctrl Pts',(2.19538337205763,3.26531526807821,298.665592096151));
#5722=CARTESIAN_POINT('Ctrl Pts',(2.09789137063639,3.32879026634996,298.671453133115));
#5723=CARTESIAN_POINT('Ctrl Pts',(1.99779351867686,3.38781789013706,298.677314170078));
#5724=CARTESIAN_POINT('Ctrl Pts',(1.89768550270672,3.44685150763315,298.683175802176));
#5725=CARTESIAN_POINT('Ctrl Pts',(1.79497146490819,3.50143664374584,298.689037434273));
#5726=CARTESIAN_POINT('Ctrl Pts',(1.69008730354519,3.55135099735232,298.694899066371));
#5727=CARTESIAN_POINT('Ctrl Pts',(1.58146358301208,3.60304500649806,298.700969690177));
#5728=CARTESIAN_POINT('Ctrl Pts',(1.47051253188316,3.64972874368019,298.707040313983));
#5729=CARTESIAN_POINT('Ctrl Pts',(1.35774128006391,3.69120950589511,298.713110937788));
#5730=CARTESIAN_POINT('Ctrl Pts',(1.24869190767526,3.73132124548092,298.718981207962));
#5731=CARTESIAN_POINT('Ctrl Pts',(1.13794100334679,3.76656795945754,298.724851478137));
#5732=CARTESIAN_POINT('Ctrl Pts',(1.02596180108698,3.79682648835977,298.730721748311));
#5733=CARTESIAN_POINT('Ctrl Pts',(0.908249786059665,3.82863411278434,298.736892548932));
#5734=CARTESIAN_POINT('Ctrl Pts',(0.78918089541764,3.85492917728933,298.743063349554));
#5735=CARTESIAN_POINT('Ctrl Pts',(0.669314601046263,3.87562987975197,298.749234150176));
#5736=CARTESIAN_POINT('Ctrl Pts',(0.549448306674884,3.89633058221461,298.755404950798));
#5737=CARTESIAN_POINT('Ctrl Pts',(0.428785134362634,3.91143692789991,298.76157575142));
#5738=CARTESIAN_POINT('Ctrl Pts',(0.307886798785825,3.92093033846987,298.767746552042));
#5739=CARTESIAN_POINT('Ctrl Pts',(0.192654567450534,3.92997882435463,298.773628147693));
#5740=CARTESIAN_POINT('Ctrl Pts',(0.0768375326098742,3.93395774820178,298.779509743344));
#5741=CARTESIAN_POINT('Ctrl Pts',(-0.0390815948845062,3.93280582141317,
298.785391338996));
#5742=CARTESIAN_POINT('Ctrl Pts',(-0.154854251100143,3.93165535015819,298.791265502873));
#5743=CARTESIAN_POINT('Ctrl Pts',(-0.270728335181155,3.9253869263451,298.797139666749));
#5744=CARTESIAN_POINT('Ctrl Pts',(-0.38621637316139,3.91399104663029,298.803013830626));
#5745=CARTESIAN_POINT('Ctrl Pts',(-0.501589080330269,3.90260654728072,298.808882128336));
#5746=CARTESIAN_POINT('Ctrl Pts',(-0.61657610078503,3.88610481820368,298.814750426046));
#5747=CARTESIAN_POINT('Ctrl Pts',(-0.730690972785378,3.86452839325706,298.820618723756));
#5748=CARTESIAN_POINT('Ctrl Pts',(-0.84699754327141,3.84253756993226,298.826599728416));
#5749=CARTESIAN_POINT('Ctrl Pts',(-0.962397683703614,3.81527511216226,298.832580733076));
#5750=CARTESIAN_POINT('Ctrl Pts',(-1.07638251898232,3.78284148132449,298.838561737737));
#5751=CARTESIAN_POINT('Ctrl Pts',(-1.18809641723311,3.75105403059515,298.844423581941));
#5752=CARTESIAN_POINT('Ctrl Pts',(-1.2984504695073,3.71429967000211,298.850285426145));
#5753=CARTESIAN_POINT('Ctrl Pts',(-1.40697760964053,3.67272419410582,298.856147270349));
#5754=CARTESIAN_POINT('Ctrl Pts',(-1.51548975614759,3.63115446209205,298.862008304707));
#5755=CARTESIAN_POINT('Ctrl Pts',(-1.6221751080147,3.58476508665275,298.867869339065));
#5756=CARTESIAN_POINT('Ctrl Pts',(-1.72658462582728,3.53375077359127,298.873730373423));
#5757=CARTESIAN_POINT('Ctrl Pts',(-1.83100476525738,3.48273127082551,298.879592004027));
#5758=CARTESIAN_POINT('Ctrl Pts',(-1.93314824039184,3.42708607590499,298.88545363463));
#5759=CARTESIAN_POINT('Ctrl Pts',(-2.03258937874266,3.36705649156983,298.891315265233));
#5760=CARTESIAN_POINT('Ctrl Pts',(-2.13557615571801,3.3048865132653,298.897385896097));
#5761=CARTESIAN_POINT('Ctrl Pts',(-2.23566388252832,3.23801389735006,298.903456526961));
#5762=CARTESIAN_POINT('Ctrl Pts',(-2.33241234216944,3.1667557004126,298.909527157825));
#5763=CARTESIAN_POINT('Ctrl Pts',(-2.42596764758634,3.09784935913677,298.915397429318));
#5764=CARTESIAN_POINT('Ctrl Pts',(-2.5164003444594,3.02484266972502,298.92126770081));
#5765=CARTESIAN_POINT('Ctrl Pts',(-2.60334692919883,2.94806271409395,298.927137972303));
#5766=CARTESIAN_POINT('Ctrl Pts',(-2.69474489998909,2.86735187118878,298.933308782853));
#5767=CARTESIAN_POINT('Ctrl Pts',(-2.78228997575694,2.78247154699177,298.939479593403));
#5768=CARTESIAN_POINT('Ctrl Pts',(-2.86560565489064,2.6938435794713,298.945650403953));
#5769=CARTESIAN_POINT('Ctrl Pts',(-2.94892133402435,2.60521561195084,298.951821214503));
#5770=CARTESIAN_POINT('Ctrl Pts',(-3.0280073312464,2.51284044281146,298.957992025052));
#5771=CARTESIAN_POINT('Ctrl Pts',(-3.10253867309009,2.41717661373355,298.964162835602));
#5772=CARTESIAN_POINT('Ctrl Pts',(-3.17357549142453,2.32599813929206,298.970044317636));
#5773=CARTESIAN_POINT('Ctrl Pts',(-3.24070398890551,2.23153863094175,298.97592579967));
#5774=CARTESIAN_POINT('Ctrl Pts',(-3.30360706473768,2.13416713539856,298.981807281704));
#5775=CARTESIAN_POINT('Ctrl Pts',(-3.36643063552401,2.03691871054967,298.98768132996));
#5776=CARTESIAN_POINT('Ctrl Pts',(-3.42503918482522,1.9367659614758,298.993555378216));
#5777=CARTESIAN_POINT('Ctrl Pts',(-3.47915620275512,1.83411044292065,298.999429426472));
#5778=CARTESIAN_POINT('Ctrl Pts',(-3.53321915928189,1.73155747438737,299.005297606716));
#5779=CARTESIAN_POINT('Ctrl Pts',(-3.58279931910324,1.62650707216866,299.011165786961));
#5780=CARTESIAN_POINT('Ctrl Pts',(-3.62766415580198,1.51938861806633,299.017033967205));
#5781=CARTESIAN_POINT('Ctrl Pts',(-3.67339191646354,1.41020986267446,299.023015015203));
#5782=CARTESIAN_POINT('Ctrl Pts',(-3.71422085474296,1.29888304458287,299.028996063201));
#5783=CARTESIAN_POINT('Ctrl Pts',(-3.74995442141005,1.18588820609162,299.0349771112));
#5784=CARTESIAN_POINT('Ctrl Pts',(-3.78497508459818,1.07514767415239,299.04083883414));
#5785=CARTESIAN_POINT('Ctrl Pts',(-3.81510167315239,0.962805470956686,299.04670055708));
#5786=CARTESIAN_POINT('Ctrl Pts',(-3.84019852157032,0.84933168722775,299.05256228002));
#5787=CARTESIAN_POINT('Ctrl Pts',(-3.8652918974921,0.735873604166504,299.058423191909));
#5788=CARTESIAN_POINT('Ctrl Pts',(-3.88535682837333,0.621284653934497,299.064284103799));
#5789=CARTESIAN_POINT('Ctrl Pts',(-3.90030839852345,0.506046832227465,299.070145015688));
#5790=CARTESIAN_POINT('Ctrl Pts',(-3.91526148700582,0.390797308117357,299.076006522753));
#5791=CARTESIAN_POINT('Ctrl Pts',(-3.92510012951962,0.274899189935423,299.081868029819));
#5792=CARTESIAN_POINT('Ctrl Pts',(-3.92979117117279,0.158840646474369,299.087729536884));
#5793=CARTESIAN_POINT('Ctrl Pts',(-3.93464971154881,0.0386381070220402,
299.093800335407));
#5794=CARTESIAN_POINT('Ctrl Pts',(-3.93398615723645,-0.0817360519541535,
299.09987113393));
#5795=CARTESIAN_POINT('Ctrl Pts',(-3.92782256344909,-0.20173970868475,299.105941932454));
#5796=CARTESIAN_POINT('Ctrl Pts',(-3.9218626888408,-0.317777003049758,299.111812078868));
#5797=CARTESIAN_POINT('Ctrl Pts',(-3.91076070600483,-0.433467489394996,
299.117682225282));
#5798=CARTESIAN_POINT('Ctrl Pts',(-3.89458930067724,-0.548327620178241,
299.123552371697));
#5799=CARTESIAN_POINT('Ctrl Pts',(-3.87758874399137,-0.669076938173299,
299.129723496275));
#5800=CARTESIAN_POINT('Ctrl Pts',(-3.85498523900164,-0.78890797412956,299.135894620852));
#5801=CARTESIAN_POINT('Ctrl Pts',(-3.8269234206086,-0.90727401197069,299.14206574543));
#5802=CARTESIAN_POINT('Ctrl Pts',(-3.79886160221556,-1.02564004981182,299.148236870008));
#5803=CARTESIAN_POINT('Ctrl Pts',(-3.76534168195458,-1.14254060791152,299.154407994585));
#5804=CARTESIAN_POINT('Ctrl Pts',(-3.72656733161276,-1.25745175770545,299.160579119163));
#5805=CARTESIAN_POINT('Ctrl Pts',(-3.68961247851761,-1.36697066962001,299.166460661992));
#5806=CARTESIAN_POINT('Ctrl Pts',(-3.64776609054497,-1.47503554147972,299.172342204821));
#5807=CARTESIAN_POINT('Ctrl Pts',(-3.60116145735301,-1.58117840804735,299.17822374765));
#5808=CARTESIAN_POINT('Ctrl Pts',(-3.55461572231055,-1.68718713305017,299.184097857484));
#5809=CARTESIAN_POINT('Ctrl Pts',(-3.50332386589151,-1.79127830985841,299.189971967319));
#5810=CARTESIAN_POINT('Ctrl Pts',(-3.44746867013671,-1.89299993883407,299.195846077153));
#5811=CARTESIAN_POINT('Ctrl Pts',(-3.3916692649337,-1.9946199639082,299.201714319676));
#5812=CARTESIAN_POINT('Ctrl Pts',(-3.33131578465535,-2.09387479039293,299.207582562199));
#5813=CARTESIAN_POINT('Ctrl Pts',(-3.26663846632172,-2.19033379427595,299.213450804722));
#5814=CARTESIAN_POINT('Ctrl Pts',(-3.20071810754434,-2.28864665428782,299.219431829638));
#5815=CARTESIAN_POINT('Ctrl Pts',(-3.1303061674118,-2.38405471685387,299.225412854555));
#5816=CARTESIAN_POINT('Ctrl Pts',(-3.05569496974759,-2.4761294901235,299.231393879472));
#5817=CARTESIAN_POINT('Ctrl Pts',(-2.98257122919138,-2.56636865050586,299.237255666013));
#5818=CARTESIAN_POINT('Ctrl Pts',(-2.90541438526128,-2.65340586242024,299.243117452554));
#5819=CARTESIAN_POINT('Ctrl Pts',(-2.82454201203783,-2.73686890848525,299.248979239095));
#5820=CARTESIAN_POINT('Ctrl Pts',(-2.74368082326022,-2.82032041182091,299.254840214965));
#5821=CARTESIAN_POINT('Ctrl Pts',(-2.65910541356834,-2.90019843665227,299.260701190836));
#5822=CARTESIAN_POINT('Ctrl Pts',(-2.57117125235045,-2.97616655970169,299.266562166706));
#5823=CARTESIAN_POINT('Ctrl Pts',(-2.48322815688645,-3.05214240122933,299.272423738061));
#5824=CARTESIAN_POINT('Ctrl Pts',(-2.39192594313031,-3.1242072820544,299.278285309416));
#5825=CARTESIAN_POINT('Ctrl Pts',(-2.29765374936215,-3.19206457454138,299.284146880771));
#5826=CARTESIAN_POINT('Ctrl Pts',(-2.20001795681944,-3.26234299139951,299.290217590933));
#5827=CARTESIAN_POINT('Ctrl Pts',(-2.09919667553962,-3.32810768099155,299.296288301096));
#5828=CARTESIAN_POINT('Ctrl Pts',(-1.99565445230437,-3.38907838608046,299.302359011259));
#5829=CARTESIAN_POINT('Ctrl Pts',(-1.89553195112258,-3.44803539223291,299.308229222139));
#5830=CARTESIAN_POINT('Ctrl Pts',(-1.79286579947545,-3.5025099374884,299.31409943302));
#5831=CARTESIAN_POINT('Ctrl Pts',(-1.68809959077946,-3.55229626743185,299.319969643901));
#5832=CARTESIAN_POINT('Ctrl Pts',(-1.5779658876126,-3.60463330388669,299.326140603704));
#5833=CARTESIAN_POINT('Ctrl Pts',(-1.46551173200654,-3.65178881422318,299.332311563508));
#5834=CARTESIAN_POINT('Ctrl Pts',(-1.35127301478791,-3.69358230441749,299.338482523312));
#5835=CARTESIAN_POINT('Ctrl Pts',(-1.23703429756927,-3.73537579461179,299.344653483115));
#5836=CARTESIAN_POINT('Ctrl Pts',(-1.12101153710817,-3.77180717586096,299.350824442919));
#5837=CARTESIAN_POINT('Ctrl Pts',(-1.00375413201564,-3.80275776804959,299.356995402723));
#5838=CARTESIAN_POINT('Ctrl Pts',(-0.891996200935767,-3.83225675061678,
299.362876939159));
#5839=CARTESIAN_POINT('Ctrl Pts',(-0.778756740685876,-3.85687246497439,
299.368758475595));
#5840=CARTESIAN_POINT('Ctrl Pts',(-0.664499721401675,-3.876458321749,299.374640012031));
#5841=CARTESIAN_POINT('Ctrl Pts',(-0.55038709765623,-3.89601942634332,299.380514115509));
#5842=CARTESIAN_POINT('Ctrl Pts',(-0.435259874857216,-3.910563246732,299.386388218987));
#5843=CARTESIAN_POINT('Ctrl Pts',(-0.319595967014109,-3.91999329308971,
299.392262322465));
#5844=CARTESIAN_POINT('Ctrl Pts',(-0.204047588459498,-3.92941392037654,
299.398130558676));
#5845=CARTESIAN_POINT('Ctrl Pts',(-0.0879639993725192,-3.9337309011422,
299.403998794888));
#5846=CARTESIAN_POINT('Ctrl Pts',(0.0281685797596234,-3.93289912546894,
299.409867031099));
#5847=CARTESIAN_POINT('Ctrl Pts',(0.14653329806966,-3.93205136255866,299.415848058398));
#5848=CARTESIAN_POINT('Ctrl Pts',(0.264948480771353,-3.92585479993738,299.421829085698));
#5849=CARTESIAN_POINT('Ctrl Pts',(0.38289547787891,-3.91431731634264,299.427810112997));
#5850=CARTESIAN_POINT('Ctrl Pts',(0.4984909030979,-3.90300986168253,299.43367189338));
#5851=CARTESIAN_POINT('Ctrl Pts',(0.613636210696612,-3.88657252532392,299.439533673764));
#5852=CARTESIAN_POINT('Ctrl Pts',(0.727845804577129,-3.86506526267791,299.445395454147));
#5853=CARTESIAN_POINT('Ctrl Pts',(0.842039604886268,-3.84356097418211,299.451256423929));
#5854=CARTESIAN_POINT('Ctrl Pts',(0.955297544220685,-3.81698822986422,299.457117393711));
#5855=CARTESIAN_POINT('Ctrl Pts',(1.06714301972724,-3.78545833096171,299.462978363493));
#5856=CARTESIAN_POINT('Ctrl Pts',(1.17899986037524,-3.75392522815882,299.468839928835));
#5857=CARTESIAN_POINT('Ctrl Pts',(1.28944355551657,-3.71743408115245,299.474701494178));
#5858=CARTESIAN_POINT('Ctrl Pts',(1.39801216353395,-3.67614621453107,299.48056305952));
#5859=CARTESIAN_POINT('Ctrl Pts',(1.51045473847569,-3.63338510594234,299.486633778417));
#5860=CARTESIAN_POINT('Ctrl Pts',(1.62088546594619,-3.58547873579373,299.492704497314));
#5861=CARTESIAN_POINT('Ctrl Pts',(1.72881451645822,-3.53266038102778,299.498775216211));
#5862=CARTESIAN_POINT('Ctrl Pts',(1.83317870714832,-3.48158659855142,299.504645421328));
#5863=CARTESIAN_POINT('Ctrl Pts',(1.93520353290518,-3.42592044474168,299.510515626445));
#5864=CARTESIAN_POINT('Ctrl Pts',(2.03447288757065,-3.36591875566538,299.516385831562));
#5865=CARTESIAN_POINT('Ctrl Pts',(2.13882848874925,-3.30284277057018,299.522556807349));
#5866=CARTESIAN_POINT('Ctrl Pts',(2.24013833689055,-3.23497549954912,299.528727783136));
#5867=CARTESIAN_POINT('Ctrl Pts',(2.33795655109297,-3.16266472538609,299.534898758922));
#5868=CARTESIAN_POINT('Ctrl Pts',(2.43577476529539,-3.09035395122306,299.541069734709));
#5869=CARTESIAN_POINT('Ctrl Pts',(2.53010098584831,-3.01360005760153,299.547240710496));
#5870=CARTESIAN_POINT('Ctrl Pts',(2.6205334766521,-2.93279615686901,299.553411686283));
#5871=CARTESIAN_POINT('Ctrl Pts',(2.70548444373599,-2.85689014731022,299.559208611219));
#5872=CARTESIAN_POINT('Ctrl Pts',(2.78729091307262,-2.77715017311055,299.565005536155));
#5873=CARTESIAN_POINT('Ctrl Pts',(2.86558028352338,-2.69387056828683,299.57080246109));
#5874=CARTESIAN_POINT('Ctrl Pts',(2.94376982409076,-2.61069715659241,299.576591994137));
#5875=CARTESIAN_POINT('Ctrl Pts',(3.01845089177533,-2.52399339245083,299.582381527184));
#5876=CARTESIAN_POINT('Ctrl Pts',(3.08928452069845,-2.43409329118112,299.588171060231));
#5877=CARTESIAN_POINT('Ctrl Pts',(3.16004045061587,-2.3442918033608,299.593954242608));
#5878=CARTESIAN_POINT('Ctrl Pts',(3.22695707589869,-2.25130128503618,299.599737424985));
#5879=CARTESIAN_POINT('Ctrl Pts',(3.28973350510711,-2.15549123528157,299.605520607363));
#5880=CARTESIAN_POINT('Ctrl Pts',(3.35247197808269,-2.05973911473071,299.61130029308));
#5881=CARTESIAN_POINT('Ctrl Pts',(3.41107499672829,-1.96117120427352,299.617079978798));
#5882=CARTESIAN_POINT('Ctrl Pts',(3.46528339540584,-1.86018815970981,299.622859664515));
#5883=CARTESIAN_POINT('Ctrl Pts',(3.51947294369267,-1.75924023091954,299.628637340409));
#5884=CARTESIAN_POINT('Ctrl Pts',(3.56927070893024,-1.65587921137128,299.634415016302));
#5885=CARTESIAN_POINT('Ctrl Pts',(3.61446258141136,-1.55053192407546,299.640192692196));
#5886=CARTESIAN_POINT('Ctrl Pts',(3.65965034692724,-1.44519421057295,299.645969843024));
#5887=CARTESIAN_POINT('Ctrl Pts',(3.70023288587998,-1.33787097926437,299.651746993851));
#5888=CARTESIAN_POINT('Ctrl Pts',(3.73604386178533,-1.22900987091891,299.657524144679));
#5889=CARTESIAN_POINT('Ctrl Pts',(3.77187742242758,-1.12008010765892,299.663304938955));
#5890=CARTESIAN_POINT('Ctrl Pts',(3.80293327544379,-1.00961093401714,299.66908573323));
#5891=CARTESIAN_POINT('Ctrl Pts',(3.82909477244069,-0.898065823682953,299.674866527506));
#5892=CARTESIAN_POINT('Ctrl Pts',(3.85526493282691,-0.786483775144647,299.680649236094));
#5893=CARTESIAN_POINT('Ctrl Pts',(3.87653742847292,-0.673825497608828,299.686431944682));
#5894=CARTESIAN_POINT('Ctrl Pts',(3.89284694541333,-0.560563698063004,299.69221465327));
#5895=CARTESIAN_POINT('Ctrl Pts',(3.90917625425363,-0.447164453232653,299.698004379281));
#5896=CARTESIAN_POINT('Ctrl Pts',(3.92053051365403,-0.333160646533695,299.703794105293));
#5897=CARTESIAN_POINT('Ctrl Pts',(3.92689638714524,-0.219029141042092,299.709583831304));
#5898=CARTESIAN_POINT('Ctrl Pts',(3.93102052731456,-0.145088883348921,299.713334713512));
#5899=CARTESIAN_POINT('Ctrl Pts',(3.9330520506215,-0.071095061957422,299.717085595719));
#5900=CARTESIAN_POINT('Ctrl Pts',(3.93299898658193,0.00282339255091775,
299.720836477927));
#5901=CARTESIAN_POINT('',(3.93299856047831,-0.00336500750684849,300.970836478009));
#5902=CARTESIAN_POINT('Ctrl Pts',(3.93299898658139,0.00282339330360925,
299.720836477965));
#5903=CARTESIAN_POINT('Ctrl Pts',(3.93286227153703,0.193268036719428,299.730500308591));
#5904=CARTESIAN_POINT('Ctrl Pts',(3.91889056996141,0.383215183348325,299.740164139217));
#5905=CARTESIAN_POINT('Ctrl Pts',(3.89131247211491,0.571118415359679,299.749827969843));
#5906=CARTESIAN_POINT('Ctrl Pts',(3.87452808318749,0.685478765531458,299.755709502814));
#5907=CARTESIAN_POINT('Ctrl Pts',(3.85267105367365,0.799282807316514,299.761591035785));
#5908=CARTESIAN_POINT('Ctrl Pts',(3.82578888170836,0.912046288626114,299.767472568755));
#5909=CARTESIAN_POINT('Ctrl Pts',(3.79894068332811,1.02466725988382,299.773346668668));
#5910=CARTESIAN_POINT('Ctrl Pts',(3.76708006784964,1.13624988898569,299.77922076858));
#5911=CARTESIAN_POINT('Ctrl Pts',(3.73030608248496,1.24631678596404,299.785094868492));
#5912=CARTESIAN_POINT('Ctrl Pts',(3.69356882892567,1.35627374229275,299.790963101042));
#5913=CARTESIAN_POINT('Ctrl Pts',(3.65192809800505,1.46471758982599,299.796831333592));
#5914=CARTESIAN_POINT('Ctrl Pts',(3.60553344841376,1.57118348781088,299.802699566141));
#5915=CARTESIAN_POINT('Ctrl Pts',(3.55824702521909,1.67969581740632,299.808680594777));
#5916=CARTESIAN_POINT('Ctrl Pts',(3.50602214080958,1.78615295067061,299.814661623413));
#5917=CARTESIAN_POINT('Ctrl Pts',(3.44906982345746,1.89008104400714,299.820642652049));
#5918=CARTESIAN_POINT('Ctrl Pts',(3.39325304405572,1.99193697769186,299.826504428558));
#5919=CARTESIAN_POINT('Ctrl Pts',(3.33289580751339,2.09136341031837,299.832366205066));
#5920=CARTESIAN_POINT('Ctrl Pts',(3.26824404288429,2.18793735654185,299.838227981575));
#5921=CARTESIAN_POINT('Ctrl Pts',(3.20360121949022,2.28449794674394,299.844088947409));
#5922=CARTESIAN_POINT('Ctrl Pts',(3.13466527817958,2.37820649296099,299.849949913244));
#5923=CARTESIAN_POINT('Ctrl Pts',(3.06172583090244,2.46866845412356,299.855810879078));
#5924=CARTESIAN_POINT('Ctrl Pts',(2.98877897275775,2.55913960649385,299.861672440404));
#5925=CARTESIAN_POINT('Ctrl Pts',(2.9118280585073,2.64636319748854,299.86753400173));
#5926=CARTESIAN_POINT('Ctrl Pts',(2.83120293986401,2.72997782285963,299.873395563056));
#5927=CARTESIAN_POINT('Ctrl Pts',(2.74770080941029,2.81657613704588,299.879466287252));
#5928=CARTESIAN_POINT('Ctrl Pts',(2.66025768621864,2.89930276628044,299.885537011448));
#5929=CARTESIAN_POINT('Ctrl Pts',(2.56928054706066,2.97779893050147,299.891607735643));
#5930=CARTESIAN_POINT('Ctrl Pts',(2.48130849086831,3.05370227318346,299.897477936608));
#5931=CARTESIAN_POINT('Ctrl Pts',(2.39003256428525,3.12565000183945,299.903348137573));
#5932=CARTESIAN_POINT('Ctrl Pts',(2.29585243996787,3.19336038897798,299.909218338538));
#5933=CARTESIAN_POINT('Ctrl Pts',(2.19684659428728,3.26454020731649,299.915389324349));
#5934=CARTESIAN_POINT('Ctrl Pts',(2.09463149365931,3.33103665683795,299.92156031016));
#5935=CARTESIAN_POINT('Ctrl Pts',(1.98970214547334,3.39257636204387,299.92773129597));
#5936=CARTESIAN_POINT('Ctrl Pts',(1.88477279728737,3.45411606724978,299.933902281781));
#5937=CARTESIAN_POINT('Ctrl Pts',(1.77712969571039,3.5106988481097,299.940073267592));
#5938=CARTESIAN_POINT('Ctrl Pts',(1.66729218737897,3.56210973468043,299.946244253403));
#5939=CARTESIAN_POINT('Ctrl Pts',(1.56260667785026,3.61110916063007,299.952125785165));
#5940=CARTESIAN_POINT('Ctrl Pts',(1.45559066607768,3.65556877395938,299.958007316927));
#5941=CARTESIAN_POINT('Ctrl Pts',(1.34667444823225,3.69526141571586,299.963888848689));
#5942=CARTESIAN_POINT('Ctrl Pts',(1.23789587840074,3.73490389402181,299.969762947388));
#5943=CARTESIAN_POINT('Ctrl Pts',(1.12722226223994,3.76979124274595,299.975637046086));
#5944=CARTESIAN_POINT('Ctrl Pts',(1.01510657011407,3.79974310333097,299.981511144785));
#5945=CARTESIAN_POINT('Ctrl Pts',(0.90310286516894,3.82966504638739,299.987379376118));
#5946=CARTESIAN_POINT('Ctrl Pts',(0.789660345262875,3.85466120232658,299.993247607451));
#5947=CARTESIAN_POINT('Ctrl Pts',(0.675249337185439,3.87460028036837,299.999115838784));
#5948=CARTESIAN_POINT('Ctrl Pts',(0.558639147709174,3.8949226226631,300.005096867875));
#5949=CARTESIAN_POINT('Ctrl Pts',(0.441023261512045,3.90999131716783,300.011077896966));
#5950=CARTESIAN_POINT('Ctrl Pts',(0.322913385621832,3.91972141170597,300.017058926056));
#5951=CARTESIAN_POINT('Ctrl Pts',(0.207158464239176,3.92925750104498,300.022920701348));
#5952=CARTESIAN_POINT('Ctrl Pts',(0.0909294984046878,3.93366587279982,300.02878247664));
#5953=CARTESIAN_POINT('Ctrl Pts',(-0.0252850199421676,3.93291872122556,
300.034644251932));
#5954=CARTESIAN_POINT('Ctrl Pts',(-0.14148346604903,3.93217167298091,300.040505216551));
#5955=CARTESIAN_POINT('Ctrl Pts',(-0.257667056951934,3.92627052199484,300.046366181171));
#5956=CARTESIAN_POINT('Ctrl Pts',(-0.373346971543809,3.9152395889446,300.052227145791));
#5957=CARTESIAN_POINT('Ctrl Pts',(-0.489038639637707,3.90420753511125,300.058088705906));
#5958=CARTESIAN_POINT('Ctrl Pts',(-0.604226119740003,3.88804470219206,300.063950266021));
#5959=CARTESIAN_POINT('Ctrl Pts',(-0.718426074681787,3.86682724920798,300.069811826136));
#5960=CARTESIAN_POINT('Ctrl Pts',(-0.836701177368185,3.84485266584044,300.075882552038));
#5961=CARTESIAN_POINT('Ctrl Pts',(-0.953916490971856,3.81745606708775,300.081953277941));
#5962=CARTESIAN_POINT('Ctrl Pts',(-1.06954837563246,3.78477942186621,300.088024003843));
#5963=CARTESIAN_POINT('Ctrl Pts',(-1.18136074768559,3.75318214034061,300.093894203617));
#5964=CARTESIAN_POINT('Ctrl Pts',(-1.29169226784869,3.71664831158494,300.099764403391));
#5965=CARTESIAN_POINT('Ctrl Pts',(-1.40008762459992,3.67535626075108,300.105634603166));
#5966=CARTESIAN_POINT('Ctrl Pts',(-1.51403716230762,3.6319484041367,300.111805592132));
#5967=CARTESIAN_POINT('Ctrl Pts',(-1.62584637717475,3.58328199783452,300.117976581099));
#5968=CARTESIAN_POINT('Ctrl Pts',(-1.73501440219533,3.52961952966248,300.124147570065));
#5969=CARTESIAN_POINT('Ctrl Pts',(-1.84418242721591,3.47595706149044,300.130318559031));
#5970=CARTESIAN_POINT('Ctrl Pts',(-1.95070883988529,3.41729884466421,300.136489547998));
#5971=CARTESIAN_POINT('Ctrl Pts',(-2.05412810537226,3.35395985764883,300.142660536964));
#5972=CARTESIAN_POINT('Ctrl Pts',(-2.15269635935121,3.29359186596465,300.148542067885));
#5973=CARTESIAN_POINT('Ctrl Pts',(-2.24875994987839,3.22877777678703,300.154423598805));
#5974=CARTESIAN_POINT('Ctrl Pts',(-2.34189223289244,3.15975153604173,300.160305129726));
#5975=CARTESIAN_POINT('Ctrl Pts',(-2.4349068152897,3.09081253068729,300.166179227565));
#5976=CARTESIAN_POINT('Ctrl Pts',(-2.5249971300413,3.01767220412538,300.172053325405));
#5977=CARTESIAN_POINT('Ctrl Pts',(-2.61176309751935,2.94060920940477,300.177927423244));
#5978=CARTESIAN_POINT('Ctrl Pts',(-2.69844239822905,2.86362318957311,300.183795653702));
#5979=CARTESIAN_POINT('Ctrl Pts',(-2.7818036509193,2.78272256780388,300.189663884159));
#5980=CARTESIAN_POINT('Ctrl Pts',(-2.86147816243415,2.69822751559473,300.195532114616));
#5981=CARTESIAN_POINT('Ctrl Pts',(-2.94268417509544,2.61210830194591,300.201513144029));
#5982=CARTESIAN_POINT('Ctrl Pts',(-3.02005989979471,2.52225530447395,300.207494173442));
#5983=CARTESIAN_POINT('Ctrl Pts',(-3.09325251614972,2.42904875853356,300.213475202855));
#5984=CARTESIAN_POINT('Ctrl Pts',(-3.16498575366242,2.3377006467889,300.219336977236));
#5985=CARTESIAN_POINT('Ctrl Pts',(-3.23270088533774,2.24313181838456,300.225198751617));
#5986=CARTESIAN_POINT('Ctrl Pts',(-3.29610557226436,2.1457346193059,300.231060525998));
#5987=CARTESIAN_POINT('Ctrl Pts',(-3.35950149032172,2.04835089026149,300.236921489696));
#5988=CARTESIAN_POINT('Ctrl Pts',(-3.41858792455225,1.94813991347986,300.242782453394));
#5989=CARTESIAN_POINT('Ctrl Pts',(-3.47311585622691,1.84552302863584,300.248643417091));
#5990=CARTESIAN_POINT('Ctrl Pts',(-3.52764932804217,1.74289571772297,300.254504976274));
#5991=CARTESIAN_POINT('Ctrl Pts',(-3.57762318335449,1.63786237646624,300.260366535457));
#5992=CARTESIAN_POINT('Ctrl Pts',(-3.62283468592864,1.53086832824783,300.266228094639));
#5993=CARTESIAN_POINT('Ctrl Pts',(-3.6696595473584,1.420056229636,300.272298821796));
#5994=CARTESIAN_POINT('Ctrl Pts',(-3.71137563291121,1.30714131369295,300.278369548953));
#5995=CARTESIAN_POINT('Ctrl Pts',(-3.74781292239943,1.19263879640729,300.28444027611));
#5996=CARTESIAN_POINT('Ctrl Pts',(-3.7830466149001,1.081918527659,300.290310474934));
#5997=CARTESIAN_POINT('Ctrl Pts',(-3.81334469339374,0.969714304558971,300.296180673759));
#5998=CARTESIAN_POINT('Ctrl Pts',(-3.83860512399242,0.856504350286162,300.302050872583));
#5999=CARTESIAN_POINT('Ctrl Pts',(-3.86515991416635,0.737493450231623,300.308221863906));
#6000=CARTESIAN_POINT('Ctrl Pts',(-3.88614702618422,0.617371542083399,300.31439285523));
#6001=CARTESIAN_POINT('Ctrl Pts',(-3.90150956439982,0.496701237059789,300.320563846553));
#6002=CARTESIAN_POINT('Ctrl Pts',(-3.91687210261542,0.376030932036179,300.326734837877));
#6003=CARTESIAN_POINT('Ctrl Pts',(-3.92661009564127,0.254812755301197,300.3329058292));
#6004=CARTESIAN_POINT('Ctrl Pts',(-3.93072991968259,0.133608751629746,300.339076820524));
#6005=CARTESIAN_POINT('Ctrl Pts',(-3.93465649713345,0.0180900054416166,
300.344958352147));
#6006=CARTESIAN_POINT('Ctrl Pts',(-3.9334926897861,-0.0977880713029246,
300.35083988377));
#6007=CARTESIAN_POINT('Ctrl Pts',(-3.92719867588365,-0.213540535116148,
300.356721415393));
#6008=CARTESIAN_POINT('Ctrl Pts',(-3.92091261634664,-0.329146711137223,
300.362595513945));
#6009=CARTESIAN_POINT('Ctrl Pts',(-3.90950926720366,-0.44462718230248,300.368469612497));
#6010=CARTESIAN_POINT('Ctrl Pts',(-3.89300075218217,-0.559494542876913,
300.37434371105));
#6011=CARTESIAN_POINT('Ctrl Pts',(-3.87650872677365,-0.67424716761256,300.380211942229));
#6012=CARTESIAN_POINT('Ctrl Pts',(-3.85492173761455,-0.788387494658678,
300.386080173408));
#6013=CARTESIAN_POINT('Ctrl Pts',(-3.82830384953644,-0.901431437006986,
300.391948404588));
#6014=CARTESIAN_POINT('Ctrl Pts',(-3.80117431773606,-1.01664828741144,300.397929433733));
#6015=CARTESIAN_POINT('Ctrl Pts',(-3.76881850597314,-1.13072573458947,300.403910462879));
#6016=CARTESIAN_POINT('Ctrl Pts',(-3.73135934974289,-1.24315984615268,300.409891492025));
#6017=CARTESIAN_POINT('Ctrl Pts',(-3.69464708088346,-1.35335216621741,300.415753267146));
#6018=CARTESIAN_POINT('Ctrl Pts',(-3.65303322709672,-1.46196566771069,300.421615042267));
#6019=CARTESIAN_POINT('Ctrl Pts',(-3.60668415290106,-1.56854021982619,300.427476817388));
#6020=CARTESIAN_POINT('Ctrl Pts',(-3.56034148873928,-1.67510003278018,300.433337781831));
#6021=CARTESIAN_POINT('Ctrl Pts',(-3.50926507071346,-1.77962107959935,300.439198746275));
#6022=CARTESIAN_POINT('Ctrl Pts',(-3.45366932690097,-1.88166340784515,300.445059710718));
#6023=CARTESIAN_POINT('Ctrl Pts',(-3.39806793441307,-1.98371610386285,300.45092127065));
#6024=CARTESIAN_POINT('Ctrl Pts',(-3.33794650035513,-2.08328921904157,300.456782830583));
#6025=CARTESIAN_POINT('Ctrl Pts',(-3.27356496741808,-2.17996821171618,300.462644390516));
#6026=CARTESIAN_POINT('Ctrl Pts',(-3.206886018671,-2.2800971353902,300.468715116647));
#6027=CARTESIAN_POINT('Ctrl Pts',(-3.1356375157091,-2.37712113013852,300.474785842777));
#6028=CARTESIAN_POINT('Ctrl Pts',(-3.06015575390324,-2.47061445026392,300.480856568908));
#6029=CARTESIAN_POINT('Ctrl Pts',(-2.98716728484268,-2.56101952481547,300.486726768487));
#6030=CARTESIAN_POINT('Ctrl Pts',(-2.91022112759993,-2.64812321743505,300.492596968066));
#6031=CARTESIAN_POINT('Ctrl Pts',(-2.82966016283104,-2.73157690041613,300.498467167645));
#6032=CARTESIAN_POINT('Ctrl Pts',(-2.74497124323042,-2.81930676150501,300.504638157051));
#6033=CARTESIAN_POINT('Ctrl Pts',(-2.65628764242745,-2.90300228752162,300.510809146458));
#6034=CARTESIAN_POINT('Ctrl Pts',(-2.5640475344818,-2.98230602737509,300.516980135864));
#6035=CARTESIAN_POINT('Ctrl Pts',(-2.47180742653616,-3.06160976722855,300.523151125271));
#6036=CARTESIAN_POINT('Ctrl Pts',(-2.37601126548068,-3.13652145545942,300.529322114677));
#6037=CARTESIAN_POINT('Ctrl Pts',(-2.27713161213382,-3.20673675580345,300.535493104084));
#6038=CARTESIAN_POINT('Ctrl Pts',(-2.18289003236026,-3.27365851983395,300.541374635529));
#6039=CARTESIAN_POINT('Ctrl Pts',(-2.08554403724696,-3.33653013104263,300.547256166974));
#6040=CARTESIAN_POINT('Ctrl Pts',(-1.98547639138279,-3.39505117770875,300.553137698419));
#6041=CARTESIAN_POINT('Ctrl Pts',(-1.88553521088857,-3.45349826554679,300.559011796792));
#6042=CARTESIAN_POINT('Ctrl Pts',(-1.78287957293349,-3.50760551789886,300.564885895165));
#6043=CARTESIAN_POINT('Ctrl Pts',(-1.67792291623876,-3.55711451701528,300.570759993538));
#6044=CARTESIAN_POINT('Ctrl Pts',(-1.57307109605039,-3.60657406380857,300.576628224537));
#6045=CARTESIAN_POINT('Ctrl Pts',(-1.46592319957269,-3.65144431931033,300.582496455535));
#6046=CARTESIAN_POINT('Ctrl Pts',(-1.35691851279621,-3.69151204110605,300.588364686534));
#6047=CARTESIAN_POINT('Ctrl Pts',(-1.24581855506076,-3.73234993835341,300.594345715747));
#6048=CARTESIAN_POINT('Ctrl Pts',(-1.13279006261636,-3.7681985473478,300.60032674496));
#6049=CARTESIAN_POINT('Ctrl Pts',(-1.01832131796954,-3.79888282174757,300.606307774173));
#6050=CARTESIAN_POINT('Ctrl Pts',(-0.906134937533447,-3.82895528992951,
300.612169549112));
#6051=CARTESIAN_POINT('Ctrl Pts',(-0.792565622134735,-3.85406734576189,
300.618031324051));
#6052=CARTESIAN_POINT('Ctrl Pts',(-0.678089027239685,-3.8741043185667,300.62389309899));
#6053=CARTESIAN_POINT('Ctrl Pts',(-0.563628264357405,-3.89413852027572,
300.629754063251));
#6054=CARTESIAN_POINT('Ctrl Pts',(-0.448260877046215,-3.90909896380426,
300.635615027512));
#6055=CARTESIAN_POINT('Ctrl Pts',(-0.332472161681067,-3.9189222066414,300.641475991772));
#6056=CARTESIAN_POINT('Ctrl Pts',(-0.216671681875719,-3.92874644754604,
300.647337551523));
#6057=CARTESIAN_POINT('Ctrl Pts',(-0.100450199251126,-3.93343241534619,
300.653199111273));
#6058=CARTESIAN_POINT('Ctrl Pts',(0.0157031198949376,-3.93296865128945,
300.659060671023));
#6059=CARTESIAN_POINT('Ctrl Pts',(0.136001308312363,-3.93248833805958,300.665131397408));
#6060=CARTESIAN_POINT('Ctrl Pts',(0.256225900979215,-3.92648389608274,300.671202123793));
#6061=CARTESIAN_POINT('Ctrl Pts',(0.375836314881207,-3.91500141307976,300.677272850178));
#6062=CARTESIAN_POINT('Ctrl Pts',(0.491495782155133,-3.90389821709722,300.683143049576));
#6063=CARTESIAN_POINT('Ctrl Pts',(0.60658059924388,-3.88767328386297,300.689013248974));
#6064=CARTESIAN_POINT('Ctrl Pts',(0.720610913084401,-3.8664206848122,300.694883448372));
#6065=CARTESIAN_POINT('Ctrl Pts',(0.840484168638869,-3.84407909728687,300.701054438251));
#6066=CARTESIAN_POINT('Ctrl Pts',(0.959191476895999,-3.81618107976652,300.707225428129));
#6067=CARTESIAN_POINT('Ctrl Pts',(1.07619311940487,-3.78289536859607,300.713396418008));
#6068=CARTESIAN_POINT('Ctrl Pts',(1.19319476191375,-3.74960965742562,300.719567407887));
#6069=CARTESIAN_POINT('Ctrl Pts',(1.30849026698904,-3.71093648525897,300.725738397765));
#6070=CARTESIAN_POINT('Ctrl Pts',(1.4215652972654,-3.66710254909932,300.731909387644));
#6071=CARTESIAN_POINT('Ctrl Pts',(1.52933639269463,-3.62532470207726,300.737790919026));
#6072=CARTESIAN_POINT('Ctrl Pts',(1.63543784988561,-3.57872467304876,300.743672450408));
#6073=CARTESIAN_POINT('Ctrl Pts',(1.73940807989206,-3.52745638266531,300.74955398179));
#6074=CARTESIAN_POINT('Ctrl Pts',(1.84324691241889,-3.47625288509938,300.755428080099));
#6075=CARTESIAN_POINT('Ctrl Pts',(1.94495950844811,-3.42039304042143,300.761302178407));
#6076=CARTESIAN_POINT('Ctrl Pts',(2.04410242477976,-3.36007950456675,300.767176276715));
#6077=CARTESIAN_POINT('Ctrl Pts',(2.14314631166475,-3.29982621321871,300.773044507648));
#6078=CARTESIAN_POINT('Ctrl Pts',(2.23962527491145,-3.23512829293464,300.778912738581));
#6079=CARTESIAN_POINT('Ctrl Pts',(2.33311933139266,-3.16623485949509,300.784780969514));
#6080=CARTESIAN_POINT('Ctrl Pts',(2.42841051739046,-3.09601716623204,300.790761998751));
#6081=CARTESIAN_POINT('Ctrl Pts',(2.5206004700145,-3.02144119401526,300.796743027988));
#6082=CARTESIAN_POINT('Ctrl Pts',(2.60927408768007,-2.94281799222469,300.802724057225));
#6083=CARTESIAN_POINT('Ctrl Pts',(2.69617966246681,-2.86576244038114,300.808585832095));
#6084=CARTESIAN_POINT('Ctrl Pts',(2.77970750466545,-2.78481984323551,300.814447606965));
#6085=CARTESIAN_POINT('Ctrl Pts',(2.85949985541869,-2.70032397627776,300.820309381835));
#6086=CARTESIAN_POINT('Ctrl Pts',(2.93928117094525,-2.6158397950397,300.826170346026));
#6087=CARTESIAN_POINT('Ctrl Pts',(3.01532773975615,-2.52780362059282,300.832031310217));
#6088=CARTESIAN_POINT('Ctrl Pts',(3.08731924326377,-2.43658549822764,300.837892274407));
#6089=CARTESIAN_POINT('Ctrl Pts',(3.1593180612869,-2.34535810787473,300.843753834086));
#6090=CARTESIAN_POINT('Ctrl Pts',(3.22726073984971,-2.25094845018128,300.849615393766));
#6091=CARTESIAN_POINT('Ctrl Pts',(3.29086821072129,-2.1537584404162,300.855476953445));
#6092=CARTESIAN_POINT('Ctrl Pts',(3.35674548210995,-2.05310025417129,300.861547679925));
#6093=CARTESIAN_POINT('Ctrl Pts',(3.41797210376408,-1.94945997571898,300.867618406405));
#6094=CARTESIAN_POINT('Ctrl Pts',(3.47428870425617,-1.84331413477952,300.873689132885));
#6095=CARTESIAN_POINT('Ctrl Pts',(3.52874506483896,-1.740674484338,300.87955933221));
#6096=CARTESIAN_POINT('Ctrl Pts',(3.57861053221662,-1.63569258843833,300.885429531534));
#6097=CARTESIAN_POINT('Ctrl Pts',(3.62369923835292,-1.52882073179313,300.891299730859));
#6098=CARTESIAN_POINT('Ctrl Pts',(3.67109830299598,-1.41647272991574,300.897470720917));
#6099=CARTESIAN_POINT('Ctrl Pts',(3.71321793158873,-1.30203644970569,300.903641710975));
#6100=CARTESIAN_POINT('Ctrl Pts',(3.74990158412522,-1.18605527247898,300.909812701032));
#6101=CARTESIAN_POINT('Ctrl Pts',(3.7865852366617,-1.07007409525226,300.91598369109));
#6102=CARTESIAN_POINT('Ctrl Pts',(3.81783284742637,-0.952548542829235,300.922154681147));
#6103=CARTESIAN_POINT('Ctrl Pts',(3.8435502305382,-0.8340327483557,300.928325671204));
#6104=CARTESIAN_POINT('Ctrl Pts',(3.87699876730369,-0.679888763662496,300.93635178284));
#6105=CARTESIAN_POINT('Ctrl Pts',(3.90118402329849,-0.523669741101071,300.944377894475));
#6106=CARTESIAN_POINT('Ctrl Pts',(3.91590394367339,-0.366313122783201,300.95240400611));
#6107=CARTESIAN_POINT('Ctrl Pts',(3.92717235235256,-0.245853321478743,300.958548163395));
#6108=CARTESIAN_POINT('Ctrl Pts',(3.93289472509772,-0.124727083469295,300.96469232068));
#6109=CARTESIAN_POINT('Ctrl Pts',(3.93299856047757,-0.00336500837822571,
300.970836477965));
#6110=CARTESIAN_POINT('',(3.93299968132247,0.00158326162505113,302.220836477997));
#6111=CARTESIAN_POINT('Ctrl Pts',(3.93299856047831,-0.00336500750684587,
300.970836478009));
#6112=CARTESIAN_POINT('Ctrl Pts',(3.93309642351835,0.111016667666786,300.976627240917));
#6113=CARTESIAN_POINT('Ctrl Pts',(3.92820031008576,0.225544572613075,300.982418003824));
#6114=CARTESIAN_POINT('Ctrl Pts',(3.91829868241434,0.339741718648166,300.988208766731));
#6115=CARTESIAN_POINT('Ctrl Pts',(3.90840490488755,0.453848327637999,300.993994938643));
#6116=CARTESIAN_POINT('Ctrl Pts',(3.89351354081032,0.567624278283278,300.999781110555));
#6117=CARTESIAN_POINT('Ctrl Pts',(3.87366511651891,0.680593538806071,301.005567282468));
#6118=CARTESIAN_POINT('Ctrl Pts',(3.85382505019857,0.793515229113815,301.011351017881));
#6119=CARTESIAN_POINT('Ctrl Pts',(3.82903214430561,0.905630487192161,301.017134753294));
#6120=CARTESIAN_POINT('Ctrl Pts',(3.79937858655754,1.01647004678349,301.022918488708));
#6121=CARTESIAN_POINT('Ctrl Pts',(3.76972992619471,1.12729130084712,301.028701268918));
#6122=CARTESIAN_POINT('Ctrl Pts',(3.73522231925427,1.23683686558601,301.034484049128));
#6123=CARTESIAN_POINT('Ctrl Pts',(3.69599851630752,1.34465012826855,301.040266829338));
#6124=CARTESIAN_POINT('Ctrl Pts',(3.65677115228748,1.45247317916388,301.046050134559));
#6125=CARTESIAN_POINT('Ctrl Pts',(3.6128268872907,1.55856321718528,301.051833439779));
#6126=CARTESIAN_POINT('Ctrl Pts',(3.56435724870095,1.66248200099521,301.057616745));
#6127=CARTESIAN_POINT('Ctrl Pts',(3.51584124399944,1.76650019363266,301.063405582536));
#6128=CARTESIAN_POINT('Ctrl Pts',(3.46279139982919,1.86834259890711,301.069194420073));
#6129=CARTESIAN_POINT('Ctrl Pts',(3.40544602109028,1.96759406317471,301.07498325761));
#6130=CARTESIAN_POINT('Ctrl Pts',(3.34807292213555,2.06689350466508,301.080774893416));
#6131=CARTESIAN_POINT('Ctrl Pts',(3.28640038253629,2.16359915404018,301.086566529223));
#6132=CARTESIAN_POINT('Ctrl Pts',(3.2207099608377,2.2573250426469,301.092358165029));
#6133=CARTESIAN_POINT('Ctrl Pts',(3.15491554705315,2.35119930525416,301.098158969361));
#6134=CARTESIAN_POINT('Ctrl Pts',(3.08509080472275,2.44208404844958,301.103959773692));
#6135=CARTESIAN_POINT('Ctrl Pts',(3.01155767267647,2.52962633290838,301.109760578024));
#6136=CARTESIAN_POINT('Ctrl Pts',(2.94825452302332,2.60498967158115,301.114754370271));
#6137=CARTESIAN_POINT('Ctrl Pts',(2.88220378713752,2.67787633476089,301.119748162518));
#6138=CARTESIAN_POINT('Ctrl Pts',(2.81363138731921,2.74808431753689,301.124741954765));
#6139=CARTESIAN_POINT('Ctrl Pts',(2.73286897173146,2.83077307128557,301.130623486196));
#6140=CARTESIAN_POINT('Ctrl Pts',(2.64832821169398,2.91003177469155,301.136505017626));
#6141=CARTESIAN_POINT('Ctrl Pts',(2.56033201258128,2.98549643867674,301.142386549057));
#6142=CARTESIAN_POINT('Ctrl Pts',(2.47244702296896,3.06086573050196,301.148260647415));
#6143=CARTESIAN_POINT('Ctrl Pts',(2.38111558943806,3.13245025346527,301.154134745773));
#6144=CARTESIAN_POINT('Ctrl Pts',(2.28669830350379,3.19992185353844,301.16000884413));
#6145=CARTESIAN_POINT('Ctrl Pts',(2.19237532678064,3.26732605924295,301.165877075113));
#6146=CARTESIAN_POINT('Ctrl Pts',(2.0949729623651,3.33062527627382,301.171745306097));
#6147=CARTESIAN_POINT('Ctrl Pts',(1.99488530741401,3.38953117853542,301.17761353708));
#6148=CARTESIAN_POINT('Ctrl Pts',(1.89287378291923,3.4495693610104,301.183594566298));
#6149=CARTESIAN_POINT('Ctrl Pts',(1.78807299843527,3.5050433050812,301.189575595517));
#6150=CARTESIAN_POINT('Ctrl Pts',(1.68093208576008,3.55569350803219,301.195556624735));
#6151=CARTESIAN_POINT('Ctrl Pts',(1.57592742985903,3.60533380882289,301.201418399657));
#6152=CARTESIAN_POINT('Ctrl Pts',(1.46867548891698,3.65034076207192,301.207280174579));
#6153=CARTESIAN_POINT('Ctrl Pts',(1.35962376252546,3.69051652541702,301.213141949501));
#6154=CARTESIAN_POINT('Ctrl Pts',(1.25058711790202,3.73068673248561,301.219002913744));
#6155=CARTESIAN_POINT('Ctrl Pts',(1.1397515691501,3.76602693607731,301.224863877987));
#6156=CARTESIAN_POINT('Ctrl Pts',(1.02758325800001,3.79638797383488,301.23072484223));
#6157=CARTESIAN_POINT('Ctrl Pts',(0.915403550261956,3.82675209635171,301.236586401962));
#6158=CARTESIAN_POINT('Ctrl Pts',(0.801891208440969,3.85213593975959,301.242447961694));
#6159=CARTESIAN_POINT('Ctrl Pts',(0.687525473407211,3.87244079663152,301.248309521426));
#6160=CARTESIAN_POINT('Ctrl Pts',(0.569078657268208,3.89347022164181,301.254380247834));
#6161=CARTESIAN_POINT('Ctrl Pts',(0.449716873291618,3.90905132129816,301.260450974243));
#6162=CARTESIAN_POINT('Ctrl Pts',(0.329980236896991,3.91913281776178,301.266521700651));
#6163=CARTESIAN_POINT('Ctrl Pts',(0.214198717309004,3.92888130423532,301.272391900029));
#6164=CARTESIAN_POINT('Ctrl Pts',(0.0980671387338737,3.93348781893126,301.278262099408));
#6165=CARTESIAN_POINT('Ctrl Pts',(-0.0179255588339876,3.93295914984385,
301.284132298786));
#6166=CARTESIAN_POINT('Ctrl Pts',(-0.139861752426486,3.93240339161475,301.290303288709));
#6167=CARTESIAN_POINT('Ctrl Pts',(-0.261643926493478,3.92617228084719,301.296474278633));
#6168=CARTESIAN_POINT('Ctrl Pts',(-0.382710894131026,3.91433536778767,301.302645268556));
#6169=CARTESIAN_POINT('Ctrl Pts',(-0.503777861768569,3.90249845472815,301.308816258479));
#6170=CARTESIAN_POINT('Ctrl Pts',(-0.624129117302728,3.88505588397538,301.314987248402));
#6171=CARTESIAN_POINT('Ctrl Pts',(-0.74321808634839,3.86213876966178,301.321158238325));
#6172=CARTESIAN_POINT('Ctrl Pts',(-0.856721028788768,3.84029661309866,301.327039769752));
#6173=CARTESIAN_POINT('Ctrl Pts',(-0.96944313299157,3.81341149870345,301.332921301179));
#6174=CARTESIAN_POINT('Ctrl Pts',(-1.08090273155306,3.78155236442934,301.338802832606));
#6175=CARTESIAN_POINT('Ctrl Pts',(-1.19222146759307,3.74973349369506,301.34467693096));
#6176=CARTESIAN_POINT('Ctrl Pts',(-1.30228047876852,3.71295321749393,301.350551029313));
#6177=CARTESIAN_POINT('Ctrl Pts',(-1.41060724030656,3.67133166760982,301.356425127667));
#6178=CARTESIAN_POINT('Ctrl Pts',(-1.51882579907708,3.62975169163434,301.362293358646));
#6179=CARTESIAN_POINT('Ctrl Pts',(-1.62531516790214,3.58334020837589,301.368161589625));
#6180=CARTESIAN_POINT('Ctrl Pts',(-1.72961760009685,3.53226725453146,301.374029820604));
#6181=CARTESIAN_POINT('Ctrl Pts',(-1.83592491773613,3.48021258415732,301.380010849824));
#6182=CARTESIAN_POINT('Ctrl Pts',(-1.93995993808061,3.42331550647589,301.385991879044));
#6183=CARTESIAN_POINT('Ctrl Pts',(-2.04125864743069,3.36180786695038,301.391972908264));
#6184=CARTESIAN_POINT('Ctrl Pts',(-2.14053758618997,3.30152661344913,301.397834683182));
#6185=CARTESIAN_POINT('Ctrl Pts',(-2.23718795307223,3.23681717642505,301.4036964581));
#6186=CARTESIAN_POINT('Ctrl Pts',(-2.33079809162441,3.16794401088151,301.409558233017));
#6187=CARTESIAN_POINT('Ctrl Pts',(-2.4243952839665,3.09908037044373,301.415419197256));
#6188=CARTESIAN_POINT('Ctrl Pts',(-2.51495275253598,3.02605439064379,301.421280161494));
#6189=CARTESIAN_POINT('Ctrl Pts',(-2.60208919539452,2.94917290425826,301.427141125733));
#6190=CARTESIAN_POINT('Ctrl Pts',(-2.68923449153746,2.87228360651801,301.433002685461));
#6191=CARTESIAN_POINT('Ctrl Pts',(-2.77295776220296,2.79153829591929,301.438864245188));
#6192=CARTESIAN_POINT('Ctrl Pts',(-2.8529125951192,2.70728253505433,301.444725804916));
#6193=CARTESIAN_POINT('Ctrl Pts',(-2.93572057434046,2.62002015152481,301.45079653133));
#6194=CARTESIAN_POINT('Ctrl Pts',(-3.01448581251665,2.52899244459817,301.456867257744));
#6195=CARTESIAN_POINT('Ctrl Pts',(-3.08886794048257,2.43462191033001,301.462937984158));
#6196=CARTESIAN_POINT('Ctrl Pts',(-3.16079309263499,2.34336860497887,301.468808183532));
#6197=CARTESIAN_POINT('Ctrl Pts',(-3.22861993213213,2.24899019989031,301.474678382906));
#6198=CARTESIAN_POINT('Ctrl Pts',(-3.29208474305109,2.15189847450344,301.48054858228));
#6199=CARTESIAN_POINT('Ctrl Pts',(-3.35880150757953,2.0498317435623,301.486719572214));
#6200=CARTESIAN_POINT('Ctrl Pts',(-3.42069711094639,1.94476672081401,301.492890562148));
#6201=CARTESIAN_POINT('Ctrl Pts',(-3.47752041045979,1.83721005735207,301.499061552082));
#6202=CARTESIAN_POINT('Ctrl Pts',(-3.53434370997318,1.72965339389013,301.505232542016));
#6203=CARTESIAN_POINT('Ctrl Pts',(-3.58609454770608,1.61960559138573,301.511403531951));
#6204=CARTESIAN_POINT('Ctrl Pts',(-3.6325812091906,1.50759502474482,301.517574521885));
#6205=CARTESIAN_POINT('Ctrl Pts',(-3.67688735191643,1.40083846288577,301.523456053319));
#6206=CARTESIAN_POINT('Ctrl Pts',(-3.71655474682514,1.29195513096818,301.529337584753));
#6207=CARTESIAN_POINT('Ctrl Pts',(-3.75137555139626,1.18138498059965,301.535219116187));
#6208=CARTESIAN_POINT('Ctrl Pts',(-3.78615234947252,1.07095456866658,301.541093214548));
#6209=CARTESIAN_POINT('Ctrl Pts',(-3.81609461649755,0.958841967506965,301.546967312909));
#6210=CARTESIAN_POINT('Ctrl Pts',(-3.84104227032977,0.845507704009778,301.55284141127));
#6211=CARTESIAN_POINT('Ctrl Pts',(-3.86596500506448,0.732286645048134,301.558709642257));
#6212=CARTESIAN_POINT('Ctrl Pts',(-3.8859029627829,0.617846751099631,301.564577873243));
#6213=CARTESIAN_POINT('Ctrl Pts',(-3.90074585091687,0.502663711197483,301.57044610423));
#6214=CARTESIAN_POINT('Ctrl Pts',(-3.91587404675698,0.385266640669798,301.576427133447));
#6215=CARTESIAN_POINT('Ctrl Pts',(-3.92570914490651,0.267097974193734,301.582408162664));
#6216=CARTESIAN_POINT('Ctrl Pts',(-3.93018898183505,0.14867268431816,301.588389191882));
#6217=CARTESIAN_POINT('Ctrl Pts',(-3.93457949638071,0.032608647598457,301.594250966807));
#6218=CARTESIAN_POINT('Ctrl Pts',(-3.93382631025829,-0.0837014439737091,
301.600112741732));
#6219=CARTESIAN_POINT('Ctrl Pts',(-3.92792332002528,-0.19976834584481,301.605974516657));
#6220=CARTESIAN_POINT('Ctrl Pts',(-3.92202114617121,-0.315819195753972,
301.611835480903));
#6221=CARTESIAN_POINT('Ctrl Pts',(-3.9109706054979,-0.431626511680904,301.61769644515));
#6222=CARTESIAN_POINT('Ctrl Pts',(-3.89481768425206,-0.546703033133568,
301.623557409396));
#6223=CARTESIAN_POINT('Ctrl Pts',(-3.87866312182813,-0.661791246654964,
301.629418969131));
#6224=CARTESIAN_POINT('Ctrl Pts',(-3.85740520550711,-0.776148110288028,
301.635280528866));
#6225=CARTESIAN_POINT('Ctrl Pts',(-3.83114146549651,-0.889294142201137,
301.641142088602));
#6226=CARTESIAN_POINT('Ctrl Pts',(-3.80394051777232,-1.00647773060195,301.647212815005));
#6227=CARTESIAN_POINT('Ctrl Pts',(-3.77136991776805,-1.12236199240654,301.653283541409));
#6228=CARTESIAN_POINT('Ctrl Pts',(-3.73359472912333,-1.23643010261903,301.659354267813));
#6229=CARTESIAN_POINT('Ctrl Pts',(-3.69706732296464,-1.34673033779912,301.665224467194));
#6230=CARTESIAN_POINT('Ctrl Pts',(-3.65567393915433,-1.4553321394044,301.671094666576));
#6231=CARTESIAN_POINT('Ctrl Pts',(-3.60961292988756,-1.56178855687592,301.676964865958));
#6232=CARTESIAN_POINT('Ctrl Pts',(-3.56119174260528,-1.67369982868355,301.683135855872));
#6233=CARTESIAN_POINT('Ctrl Pts',(-3.50761215158859,-1.7832395568609,301.689306845787));
#6234=CARTESIAN_POINT('Ctrl Pts',(-3.44915861034888,-1.8899190143115,301.695477835701));
#6235=CARTESIAN_POINT('Ctrl Pts',(-3.39070506910917,-1.9965984717621,301.701648825616));
#6236=CARTESIAN_POINT('Ctrl Pts',(-3.32737790930106,-2.10041725029467,301.707819815531));
#6237=CARTESIAN_POINT('Ctrl Pts',(-3.25951245570123,-2.20092424929359,301.713990805445));
#6238=CARTESIAN_POINT('Ctrl Pts',(-3.19483032139855,-2.29671683392642,301.719872336876));
#6239=CARTESIAN_POINT('Ctrl Pts',(-3.12581760277878,-2.38980994238618,301.725753868308));
#6240=CARTESIAN_POINT('Ctrl Pts',(-3.05272694618447,-2.47978773124621,301.731635399739));
#6241=CARTESIAN_POINT('Ctrl Pts',(-2.97972866148265,-2.56965180627432,301.737509498097));
#6242=CARTESIAN_POINT('Ctrl Pts',(-2.90266294612174,-2.65640807518584,301.743383596455));
#6243=CARTESIAN_POINT('Ctrl Pts',(-2.82182593083418,-2.73966921654272,301.749257694813));
#6244=CARTESIAN_POINT('Ctrl Pts',(-2.74106966003229,-2.82284719206264,301.755125925797));
#6245=CARTESIAN_POINT('Ctrl Pts',(-2.65654986806582,-2.90253669097835,301.76099415678));
#6246=CARTESIAN_POINT('Ctrl Pts',(-2.56860277056359,-2.97838358964272,301.766862387764));
#6247=CARTESIAN_POINT('Ctrl Pts',(-2.47896516745751,-3.05568840574687,301.772843416982));
#6248=CARTESIAN_POINT('Ctrl Pts',(-2.38576741288062,-3.12900103385473,301.778824446201));
#6249=CARTESIAN_POINT('Ctrl Pts',(-2.28940502271977,-3.19798587269323,301.784805475419));
#6250=CARTESIAN_POINT('Ctrl Pts',(-2.19496397897023,-3.26559523950041,301.790667250341));
#6251=CARTESIAN_POINT('Ctrl Pts',(-2.09748367848344,-3.32904754989868,301.796529025264));
#6252=CARTESIAN_POINT('Ctrl Pts',(-1.99736905234712,-3.38806816175914,301.802390800186));
#6253=CARTESIAN_POINT('Ctrl Pts',(-1.89726827198561,-3.44708061111496,301.808251764429));
#6254=CARTESIAN_POINT('Ctrl Pts',(-1.79453424516427,-3.5016623717278,301.814112728672));
#6255=CARTESIAN_POINT('Ctrl Pts',(-1.68959894593133,-3.55158336547345,301.819973692915));
#6256=CARTESIAN_POINT('Ctrl Pts',(-1.58465298500382,-3.60150943131964,301.825835252648));
#6257=CARTESIAN_POINT('Ctrl Pts',(-1.4775056789278,-3.64677361201657,301.83169681238));
#6258=CARTESIAN_POINT('Ctrl Pts',(-1.36861090822361,-3.68719313053864,301.837558372112));
#6259=CARTESIAN_POINT('Ctrl Pts',(-1.25583028490971,-3.72905499831694,301.84362909852));
#6260=CARTESIAN_POINT('Ctrl Pts',(-1.14117559858218,-3.76571981855612,301.849699824928));
#6261=CARTESIAN_POINT('Ctrl Pts',(-1.02516910154362,-3.79704059936686,301.855770551336));
#6262=CARTESIAN_POINT('Ctrl Pts',(-0.912994508079964,-3.82732679836519,
301.861640750714));
#6263=CARTESIAN_POINT('Ctrl Pts',(-0.799556420831486,-3.85261639866851,
301.867510950093));
#6264=CARTESIAN_POINT('Ctrl Pts',(-0.685337119421168,-3.8728286862116,301.873381149471));
#6265=CARTESIAN_POINT('Ctrl Pts',(-0.56526519128116,-3.89407665662863,301.879552139394));
#6266=CARTESIAN_POINT('Ctrl Pts',(-0.444330394377407,-3.90971313830002,
301.885723129316));
#6267=CARTESIAN_POINT('Ctrl Pts',(-0.323097309888554,-3.9197062553644,301.891894119239));
#6268=CARTESIAN_POINT('Ctrl Pts',(-0.201864225399701,-3.92969937242878,
301.898065109161));
#6269=CARTESIAN_POINT('Ctrl Pts',(-0.080333376702017,-3.93404917677253,
301.904236099084));
#6270=CARTESIAN_POINT('Ctrl Pts',(0.0409340283513448,-3.93278697685534,
301.910407089006));
#6271=CARTESIAN_POINT('Ctrl Pts',(0.156513224452326,-3.93158398210432,301.916288620437));
#6272=CARTESIAN_POINT('Ctrl Pts',(0.27222553085449,-3.92527967244625,301.922170151868));
#6273=CARTESIAN_POINT('Ctrl Pts',(0.387584714775992,-3.91385578284024,301.928051683299));
#6274=CARTESIAN_POINT('Ctrl Pts',(0.502798107885911,-3.90244633073353,301.933925781657));
#6275=CARTESIAN_POINT('Ctrl Pts',(0.617658859821588,-3.88593020698826,301.939799880015));
#6276=CARTESIAN_POINT('Ctrl Pts',(0.731680582858796,-3.86434115014027,301.945673978373));
#6277=CARTESIAN_POINT('Ctrl Pts',(0.845588414687085,-3.84277365763737,301.951542209357));
#6278=CARTESIAN_POINT('Ctrl Pts',(0.958658482398417,-3.81614338804519,301.95741044034));
#6279=CARTESIAN_POINT('Ctrl Pts',(1.07041001841268,-3.78453582259195,301.963278671323));
#6280=CARTESIAN_POINT('Ctrl Pts',(1.18430962529593,-3.75232070136803,301.969259700542));
#6281=CARTESIAN_POINT('Ctrl Pts',(1.29683905491361,-3.71493500399106,301.97524072976));
#6282=CARTESIAN_POINT('Ctrl Pts',(1.40750032594332,-3.67252390495548,301.981221758979));
#6283=CARTESIAN_POINT('Ctrl Pts',(1.51595514862774,-3.63095843057627,301.987083533901));
#6284=CARTESIAN_POINT('Ctrl Pts',(1.62261521870239,-3.58456625312263,301.992945308823));
#6285=CARTESIAN_POINT('Ctrl Pts',(1.72702824035086,-3.53353398979416,301.998807083745));
#6286=CARTESIAN_POINT('Ctrl Pts',(1.83142682175967,-3.482508784188,302.004668047988));
#6287=CARTESIAN_POINT('Ctrl Pts',(1.93357860287773,-3.42684494967813,302.010529012231));
#6288=CARTESIAN_POINT('Ctrl Pts',(2.03305357901926,-3.3667762243483,302.016389976474));
#6289=CARTESIAN_POINT('Ctrl Pts',(2.13253866207282,-3.30670139588231,302.022251536206));
#6290=CARTESIAN_POINT('Ctrl Pts',(2.22934604697387,-3.24222099977867,302.028113095938));
#6291=CARTESIAN_POINT('Ctrl Pts',(2.32307313432031,-3.17361311640206,302.03397465567));
#6292=CARTESIAN_POINT('Ctrl Pts',(2.42014482348011,-3.10255699679354,302.040045382078));
#6293=CARTESIAN_POINT('Ctrl Pts',(2.51391188487007,-3.02707359239515,302.046116108486));
#6294=CARTESIAN_POINT('Ctrl Pts',(2.60396391385506,-2.94751775827401,302.052186834894));
#6295=CARTESIAN_POINT('Ctrl Pts',(2.69104136209466,-2.8705897966731,302.058057034272));
#6296=CARTESIAN_POINT('Ctrl Pts',(2.77464507276988,-2.78985453124993,302.063927233651));
#6297=CARTESIAN_POINT('Ctrl Pts',(2.8544419755787,-2.70566997397213,302.069797433029));
#6298=CARTESIAN_POINT('Ctrl Pts',(2.93832769246227,-2.61717177806229,302.075968422952));
#6299=CARTESIAN_POINT('Ctrl Pts',(3.0180057981482,-2.52486184285586,302.082139412875));
#6300=CARTESIAN_POINT('Ctrl Pts',(3.09313863581024,-2.42919377153367,302.088310402798));
#6301=CARTESIAN_POINT('Ctrl Pts',(3.16827147347228,-2.33352570021148,302.09448139272));
#6302=CARTESIAN_POINT('Ctrl Pts',(3.23885879805826,-2.23449995813827,302.100652382643));
#6303=CARTESIAN_POINT('Ctrl Pts',(3.30461754106501,-2.13260214463116,302.106823372566));
#6304=CARTESIAN_POINT('Ctrl Pts',(3.36854554677612,-2.03354118777613,302.112822560826));
#6305=CARTESIAN_POINT('Ctrl Pts',(3.42811017090977,-1.93145696754079,302.118821749086));
#6306=CARTESIAN_POINT('Ctrl Pts',(3.48302060674435,-1.82676119210864,302.124820937346));
#6307=CARTESIAN_POINT('Ctrl Pts',(3.5378536738083,-1.72221293296029,302.130811672753));
#6308=CARTESIAN_POINT('Ctrl Pts',(3.58804542311245,-1.6150607833623,302.13680240816));
#6309=CARTESIAN_POINT('Ctrl Pts',(3.63334843404784,-1.50574505039935,302.142793143567));
#6310=CARTESIAN_POINT('Ctrl Pts',(3.67859675921488,-1.39656127367341,302.148776647491));
#6311=CARTESIAN_POINT('Ctrl Pts',(3.71896794345594,-1.28521946973946,302.154760151415));
#6312=CARTESIAN_POINT('Ctrl Pts',(3.75426080001111,-1.17218379339589,302.160743655339));
#6313=CARTESIAN_POINT('Ctrl Pts',(3.78951057542934,-1.05928609697023,302.166719855345));
#6314=CARTESIAN_POINT('Ctrl Pts',(3.81969425795302,-0.944699018097502,302.17269605535));
#6315=CARTESIAN_POINT('Ctrl Pts',(3.84465930220239,-0.828905211703131,302.178672255355));
#6316=CARTESIAN_POINT('Ctrl Pts',(3.86960642744596,-0.71319451791486,302.18464416586));
#6317=CARTESIAN_POINT('Ctrl Pts',(3.88934228772551,-0.596279200328868,302.190616076365));
#6318=CARTESIAN_POINT('Ctrl Pts',(3.90376457098115,-0.478655590537035,302.19658798687));
#6319=CARTESIAN_POINT('Ctrl Pts',(3.91817850501867,-0.36110007434428,302.202556440171));
#6320=CARTESIAN_POINT('Ctrl Pts',(3.92728494152255,-0.242837468855173,302.208524893471));
#6321=CARTESIAN_POINT('Ctrl Pts',(3.93103301119697,-0.124372283406156,302.214493346772));
#6322=CARTESIAN_POINT('Ctrl Pts',(3.9323607978372,-0.0824049497558171,302.216607723836));
#6323=CARTESIAN_POINT('Ctrl Pts',(3.93301658695605,-0.0404122476420527,
302.218722100901));
#6324=CARTESIAN_POINT('Ctrl Pts',(3.93299968132272,0.00158326098779867,
302.220836477965));
#6325=CARTESIAN_POINT('',(3.93299980390471,0.00124196841146249,303.470836477931));
#6326=CARTESIAN_POINT('Ctrl Pts',(3.93299968132247,0.00158326162505384,
302.220836477997));
#6327=CARTESIAN_POINT('Ctrl Pts',(3.93294868380391,0.128266824884077,302.227214703415));
#6328=CARTESIAN_POINT('Ctrl Pts',(3.92677272985102,0.254761136096585,302.233592928833));
#6329=CARTESIAN_POINT('Ctrl Pts',(3.91455140815298,0.380494773850481,302.239971154252));
#6330=CARTESIAN_POINT('Ctrl Pts',(3.90227516682082,0.5067934278565,302.246378041856));
#6331=CARTESIAN_POINT('Ctrl Pts',(3.88389919273337,0.632324281556489,302.252784929461));
#6332=CARTESIAN_POINT('Ctrl Pts',(3.85955466376678,0.756522833360689,302.259191817066));
#6333=CARTESIAN_POINT('Ctrl Pts',(3.83515314991891,0.881012105093762,302.265613701705));
#6334=CARTESIAN_POINT('Ctrl Pts',(3.80475523229135,1.00416257072053,302.272035586344));
#6335=CARTESIAN_POINT('Ctrl Pts',(3.7685419950764,1.1254244671881,302.278457470983));
#6336=CARTESIAN_POINT('Ctrl Pts',(3.73221410263239,1.24707029261601,302.284899688039));
#6337=CARTESIAN_POINT('Ctrl Pts',(3.69003414469865,1.36681531903206,302.291341905096));
#6338=CARTESIAN_POINT('Ctrl Pts',(3.64223220348205,1.4841272101536,302.297784122152));
#6339=CARTESIAN_POINT('Ctrl Pts',(3.6287386544955,1.51724205254839,302.299602633477));
#6340=CARTESIAN_POINT('Ctrl Pts',(3.61479741450538,1.55016316822392,302.301421144801));
#6341=CARTESIAN_POINT('Ctrl Pts',(3.60041431324821,1.58287895082266,302.303239656125));
#6342=CARTESIAN_POINT('Ctrl Pts',(3.55389567958219,1.68869017182401,302.309121187556));
#6343=CARTESIAN_POINT('Ctrl Pts',(3.50263369698545,1.79261943292796,302.315002718987));
#6344=CARTESIAN_POINT('Ctrl Pts',(3.44680261578071,1.8942124294406,302.320884250418));
#6345=CARTESIAN_POINT('Ctrl Pts',(3.39104209383576,1.99567703283458,302.326758348776));
#6346=CARTESIAN_POINT('Ctrl Pts',(3.33072415434759,2.09481088605764,302.332632447134));
#6347=CARTESIAN_POINT('Ctrl Pts',(3.26607092977507,2.19117997473467,302.338506545492));
#6348=CARTESIAN_POINT('Ctrl Pts',(3.20148228442225,2.28745280463124,302.344374776475));
#6349=CARTESIAN_POINT('Ctrl Pts',(3.13256719626738,2.38096602345876,302.350243007459));
#6350=CARTESIAN_POINT('Ctrl Pts',(3.0595931709049,2.47131111528924,302.356111238442));
#6351=CARTESIAN_POINT('Ctrl Pts',(2.98521645002923,2.56339280660589,302.362092267661));
#6352=CARTESIAN_POINT('Ctrl Pts',(2.90662334810156,2.65218293684626,302.368073296879));
#6353=CARTESIAN_POINT('Ctrl Pts',(2.82414302670637,2.73728061489972,302.374054326098));
#6354=CARTESIAN_POINT('Ctrl Pts',(2.74330726051104,2.82068155091131,302.37991610102));
#6355=CARTESIAN_POINT('Ctrl Pts',(2.65873815131185,2.90053560808156,302.385777875942));
#6356=CARTESIAN_POINT('Ctrl Pts',(2.57078502006563,2.97650018992207,302.391639650864));
#6357=CARTESIAN_POINT('Ctrl Pts',(2.48284405266891,3.05245426592013,302.397500615107));
#6358=CARTESIAN_POINT('Ctrl Pts',(2.39152030552604,3.12451966722851,302.40336157935));
#6359=CARTESIAN_POINT('Ctrl Pts',(2.29719767240265,3.19239281008898,302.409222543593));
#6360=CARTESIAN_POINT('Ctrl Pts',(2.20286545585876,3.26027284903418,302.415084103325));
#6361=CARTESIAN_POINT('Ctrl Pts',(2.10553408188791,3.32395954225861,302.420945663057));
#6362=CARTESIAN_POINT('Ctrl Pts',(2.00561745251773,3.38319192984322,302.426807222789));
#6363=CARTESIAN_POINT('Ctrl Pts',(1.90213535078178,3.44453799402423,302.432877949197));
#6364=CARTESIAN_POINT('Ctrl Pts',(1.79588044885773,3.50110566993879,302.438948675605));
#6365=CARTESIAN_POINT('Ctrl Pts',(1.68734031573658,3.5526569858192,302.445019402014));
#6366=CARTESIAN_POINT('Ctrl Pts',(1.58238545874658,3.60250546886682,302.450889601392));
#6367=CARTESIAN_POINT('Ctrl Pts',(1.47529436655552,3.64766365189985,302.45675980077));
#6368=CARTESIAN_POINT('Ctrl Pts',(1.36652712562125,3.68796591835409,302.462630000149));
#6369=CARTESIAN_POINT('Ctrl Pts',(1.25218662294444,3.73033328343396,302.468800990072));
#6370=CARTESIAN_POINT('Ctrl Pts',(1.13599415365427,3.76733375293837,302.474971979995));
#6371=CARTESIAN_POINT('Ctrl Pts',(1.01849950972216,3.7988350515251,302.481142969918));
#6372=CARTESIAN_POINT('Ctrl Pts',(0.901004865790038,3.83033635011184,302.487313959841));
#6373=CARTESIAN_POINT('Ctrl Pts',(0.782208571438175,3.85633843528387,302.493484949763));
#6374=CARTESIAN_POINT('Ctrl Pts',(0.662668393150532,3.87677180147598,302.499655939686));
#6375=CARTESIAN_POINT('Ctrl Pts',(0.548735405950958,3.89624671344413,302.505537471118));
#6376=CARTESIAN_POINT('Ctrl Pts',(0.433759646994256,3.91072625163266,302.511419002549));
#6377=CARTESIAN_POINT('Ctrl Pts',(0.318216254326758,3.92010553626841,302.51730053398));
#6378=CARTESIAN_POINT('Ctrl Pts',(0.202818885273631,3.92947296737441,302.523174632338));
#6379=CARTESIAN_POINT('Ctrl Pts',(0.0868557161750379,3.93375293139621,302.529048730696));
#6380=CARTESIAN_POINT('Ctrl Pts',(-0.0291886673971811,3.93289168700278,
302.534922829054));
#6381=CARTESIAN_POINT('Ctrl Pts',(-0.145117139415065,3.93203130286793,302.540791060038));
#6382=CARTESIAN_POINT('Ctrl Pts',(-0.261126255042839,3.92603992884984,302.546659291022));
#6383=CARTESIAN_POINT('Ctrl Pts',(-0.376727709900703,3.91491573761083,302.552527522005));
#6384=CARTESIAN_POINT('Ctrl Pts',(-0.494551238172591,3.90357771887601,302.558508551223));
#6385=CARTESIAN_POINT('Ctrl Pts',(-0.611950838548064,3.88690748403242,302.564489580442));
#6386=CARTESIAN_POINT('Ctrl Pts',(-0.728410600579572,3.86495886096648,302.57047060966));
#6387=CARTESIAN_POINT('Ctrl Pts',(-0.84254829955899,3.84344786619186,302.576332384582));
#6388=CARTESIAN_POINT('Ctrl Pts',(-0.955782868850262,3.81686710255979,302.582194159504));
#6389=CARTESIAN_POINT('Ctrl Pts',(-1.06763594037816,3.78531933907997,302.588055934427));
#6390=CARTESIAN_POINT('Ctrl Pts',(-1.17947354271327,3.75377593863131,302.59391689867));
#6391=CARTESIAN_POINT('Ctrl Pts',(-1.2899296310067,3.71726701619518,302.599777862913));
#6392=CARTESIAN_POINT('Ctrl Pts',(-1.39853934699871,3.67594568715268,302.605638827156));
#6393=CARTESIAN_POINT('Ctrl Pts',(-1.50716009801522,3.63462015975763,302.611500386888));
#6394=CARTESIAN_POINT('Ctrl Pts',(-1.61393371891148,3.58848140019214,302.617361946621));
#6395=CARTESIAN_POINT('Ctrl Pts',(-1.71841438968569,3.53773105045044,302.623223506353));
#6396=CARTESIAN_POINT('Ctrl Pts',(-1.8266233982354,3.48516970117496,302.62929423276));
#6397=CARTESIAN_POINT('Ctrl Pts',(-1.93237232452447,3.42766169539494,302.635364959168));
#6398=CARTESIAN_POINT('Ctrl Pts',(-2.03519394636018,3.36548281836334,302.641435685576));
#6399=CARTESIAN_POINT('Ctrl Pts',(-2.13461918480063,3.30535782165104,302.647305884955));
#6400=CARTESIAN_POINT('Ctrl Pts',(-2.23130713953885,3.24086593897765,302.653176084333));
#6401=CARTESIAN_POINT('Ctrl Pts',(-2.32486611309871,3.17229988433712,302.659046283712));
#6402=CARTESIAN_POINT('Ctrl Pts',(-2.42321907281232,3.10022048721262,302.665217273634));
#6403=CARTESIAN_POINT('Ctrl Pts',(-2.5181134859288,3.02363866808636,302.671388263556));
#6404=CARTESIAN_POINT('Ctrl Pts',(-2.60913605640904,2.94294037301918,302.677559253479));
#6405=CARTESIAN_POINT('Ctrl Pts',(-2.70015862688927,2.86224207795201,302.683730243401));
#6406=CARTESIAN_POINT('Ctrl Pts',(-2.78730903044837,2.77742772101423,302.689901233324));
#6407=CARTESIAN_POINT('Ctrl Pts',(-2.87022196134231,2.68892448622647,302.696072223246));
#6408=CARTESIAN_POINT('Ctrl Pts',(-2.94924575095883,2.60457261335401,302.70195375468));
#6409=CARTESIAN_POINT('Ctrl Pts',(-3.02467521876955,2.51659831271189,302.707835286115));
#6410=CARTESIAN_POINT('Ctrl Pts',(-3.09616106188238,2.42534032228126,302.713716817549));
#6411=CARTESIAN_POINT('Ctrl Pts',(-3.16755656126438,2.33419766359975,302.71959091591));
#6412=CARTESIAN_POINT('Ctrl Pts',(-3.23501809650283,2.23977989008139,302.725465014271));
#6413=CARTESIAN_POINT('Ctrl Pts',(-3.29823383664126,2.14246179868736,302.731339112632));
#6414=CARTESIAN_POINT('Ctrl Pts',(-3.36138643339906,2.04524091399017,302.737207343619));
#6415=CARTESIAN_POINT('Ctrl Pts',(-3.42030144830607,1.94512581771063,302.743075574605));
#6416=CARTESIAN_POINT('Ctrl Pts',(-3.47470832579785,1.84252301223922,302.748943805592));
#6417=CARTESIAN_POINT('Ctrl Pts',(-3.53016100389512,1.73794799147018,302.754924834809));
#6418=CARTESIAN_POINT('Ctrl Pts',(-3.58093017604073,1.63078897854424,302.760905864027));
#6419=CARTESIAN_POINT('Ctrl Pts',(-3.62677652361598,1.5215061773611,302.766886893244));
#6420=CARTESIAN_POINT('Ctrl Pts',(-3.6717087519777,1.41440233946629,302.772748668169));
#6421=CARTESIAN_POINT('Ctrl Pts',(-3.71191248138543,1.30525901703019,302.778610443094));
#6422=CARTESIAN_POINT('Ctrl Pts',(-3.74720992042188,1.19453204741096,302.78447221802));
#6423=CARTESIAN_POINT('Ctrl Pts',(-3.78250247784995,1.08382039124556,302.790333182266));
#6424=CARTESIAN_POINT('Ctrl Pts',(-3.81288996927061,0.97152591570686,302.796194146512));
#6425=CARTESIAN_POINT('Ctrl Pts',(-3.83824406250132,0.858120921941285,302.802055110759));
#6426=CARTESIAN_POINT('Ctrl Pts',(-3.86360073177262,0.744704405938851,302.807916670494));
#6427=CARTESIAN_POINT('Ctrl Pts',(-3.88392289636919,0.630177549295771,302.813778230229));
#6428=CARTESIAN_POINT('Ctrl Pts',(-3.89913321057087,0.515023500651496,302.819639789964));
#6429=CARTESIAN_POINT('Ctrl Pts',(-3.91488629681441,0.395760240502265,302.825710516368));
#6430=CARTESIAN_POINT('Ctrl Pts',(-3.92515582547606,0.275824662378546,302.831781242771));
#6431=CARTESIAN_POINT('Ctrl Pts',(-3.92991453478782,0.155758625004988,302.837851969175));
#6432=CARTESIAN_POINT('Ctrl Pts',(-3.93451605536408,0.0396585849962591,
302.843722168557));
#6433=CARTESIAN_POINT('Ctrl Pts',(-3.9339651358796,-0.0765630137847103,
302.849592367938));
#6434=CARTESIAN_POINT('Ctrl Pts',(-3.92829025249607,-0.192418014084886,
302.85546256732));
#6435=CARTESIAN_POINT('Ctrl Pts',(-3.92232458662173,-0.314209454534326,
302.861633557234));
#6436=CARTESIAN_POINT('Ctrl Pts',(-3.9106959918333,-0.435595204961309,302.867804547149));
#6437=CARTESIAN_POINT('Ctrl Pts',(-3.89349885041236,-0.55601771719759,302.873975537064));
#6438=CARTESIAN_POINT('Ctrl Pts',(-3.87630170899142,-0.676440229433871,
302.880146526978));
#6439=CARTESIAN_POINT('Ctrl Pts',(-3.8535361878316,-0.795899004719565,302.886317516893));
#6440=CARTESIAN_POINT('Ctrl Pts',(-3.82535752409154,-0.913853824676704,
302.892488506807));
#6441=CARTESIAN_POINT('Ctrl Pts',(-3.7985006180461,-1.02627581694782,302.898370038234));
#6442=CARTESIAN_POINT('Ctrl Pts',(-3.76664036763767,-1.13769397793619,302.90425156966));
#6443=CARTESIAN_POINT('Ctrl Pts',(-3.7298670150836,-1.24763017348545,302.910133101087));
#6444=CARTESIAN_POINT('Ctrl Pts',(-3.69314013665257,-1.35742743179014,302.91600719944));
#6445=CARTESIAN_POINT('Ctrl Pts',(-3.65151263467761,-1.46574606241026,302.921881297793));
#6446=CARTESIAN_POINT('Ctrl Pts',(-3.60512548911715,-1.57211933634754,302.927755396147));
#6447=CARTESIAN_POINT('Ctrl Pts',(-3.55878467760544,-1.67838635877052,302.933623627126));
#6448=CARTESIAN_POINT('Ctrl Pts',(-3.50769384352709,-1.78271151453597,302.939491858104));
#6449=CARTESIAN_POINT('Ctrl Pts',(-3.45204316688148,-1.88464505251968,302.945360089083));
#6450=CARTESIAN_POINT('Ctrl Pts',(-3.39532278141245,-1.98853794143234,302.951341118303));
#6451=CARTESIAN_POINT('Ctrl Pts',(-3.33386558241127,-2.08994590758986,302.957322147524));
#6452=CARTESIAN_POINT('Ctrl Pts',(-3.26792377584389,-2.18841568155463,302.963303176744));
#6453=CARTESIAN_POINT('Ctrl Pts',(-3.20329676709277,-2.28492209038707,302.969164951661));
#6454=CARTESIAN_POINT('Ctrl Pts',(-3.13436256896134,-2.37860603237821,302.975026726579));
#6455=CARTESIAN_POINT('Ctrl Pts',(-3.06140364168512,-2.46906799069549,302.980888501496));
#6456=CARTESIAN_POINT('Ctrl Pts',(-2.98845480457132,-2.5595174381949,302.986749465735));
#6457=CARTESIAN_POINT('Ctrl Pts',(-2.91148260371394,-2.64674546771949,302.992610429974));
#6458=CARTESIAN_POINT('Ctrl Pts',(-2.83081048851824,-2.73038476740827,302.998471394212));
#6459=CARTESIAN_POINT('Ctrl Pts',(-2.75013017682898,-2.81403256506416,303.00433295394));
#6460=CARTESIAN_POINT('Ctrl Pts',(-2.66574948938785,-2.89409061163836,303.010194513667));
#6461=CARTESIAN_POINT('Ctrl Pts',(-2.57802901917495,-2.97022816906241,303.016056073395));
#6462=CARTESIAN_POINT('Ctrl Pts',(-2.48717828995853,-3.04908265531795,303.022126799809));
#6463=CARTESIAN_POINT('Ctrl Pts',(-2.39274532702639,-3.12373131025878,303.028197526224));
#6464=CARTESIAN_POINT('Ctrl Pts',(-2.29516731291136,-3.1938528466013,303.034268252638));
#6465=CARTESIAN_POINT('Ctrl Pts',(-2.20081247655511,-3.26165814215536,303.040138452012));
#6466=CARTESIAN_POINT('Ctrl Pts',(-2.10351746537417,-3.32523049700737,303.046008651386));
#6467=CARTESIAN_POINT('Ctrl Pts',(-2.00370535464323,-3.38432472611214,303.05187885076));
#6468=CARTESIAN_POINT('Ctrl Pts',(-1.89877884509945,-3.44644695906301,303.058049840695));
#6469=CARTESIAN_POINT('Ctrl Pts',(-1.79107091742452,-3.50361974134971,303.064220830629));
#6470=CARTESIAN_POINT('Ctrl Pts',(-1.68109886722032,-3.55561465834398,303.070391820564));
#6471=CARTESIAN_POINT('Ctrl Pts',(-1.57112681701613,-3.60760957533824,303.076562810498));
#6472=CARTESIAN_POINT('Ctrl Pts',(-1.45889115246716,-3.65442649152831,303.082733800432));
#6473=CARTESIAN_POINT('Ctrl Pts',(-1.34492823469066,-3.69589732589149,303.088904790367));
#6474=CARTESIAN_POINT('Ctrl Pts',(-1.23631089938228,-3.73542291552563,303.094786321798));
#6475=CARTESIAN_POINT('Ctrl Pts',(-1.12577471544002,-3.77021995865531,303.100667853229));
#6476=CARTESIAN_POINT('Ctrl Pts',(-1.01376842338987,-3.80010033864076,303.106549384661));
#6477=CARTESIAN_POINT('Ctrl Pts',(-0.9019036847711,-3.82994295583413,303.112423483019));
#6478=CARTESIAN_POINT('Ctrl Pts',(-0.788572927624629,-3.85488116269695,
303.118297581377));
#6479=CARTESIAN_POINT('Ctrl Pts',(-0.674243328308384,-3.87477546887967,
303.124171679735));
#6480=CARTESIAN_POINT('Ctrl Pts',(-0.560027927725882,-3.8946499035279,303.130039910718));
#6481=CARTESIAN_POINT('Ctrl Pts',(-0.444816073096787,-3.90949038943808,
303.135908141702));
#6482=CARTESIAN_POINT('Ctrl Pts',(-0.32908787876733,-3.91920784955945,303.141776372685));
#6483=CARTESIAN_POINT('Ctrl Pts',(-0.211135174855228,-3.92911209720727,
303.147757401904));
#6484=CARTESIAN_POINT('Ctrl Pts',(-0.0926464960115012,-3.93369422362778,
303.153738431122));
#6485=CARTESIAN_POINT('Ctrl Pts',(0.0258609341336898,-3.93291497646284,
303.15971946034));
#6486=CARTESIAN_POINT('Ctrl Pts',(0.142005473262988,-3.93215126651885,303.165581235262));
#6487=CARTESIAN_POINT('Ctrl Pts',(0.258167592750564,-3.9262380041259,303.171443010184));
#6488=CARTESIAN_POINT('Ctrl Pts',(0.373858259076704,-3.91519080021908,303.177304785106));
#6489=CARTESIAN_POINT('Ctrl Pts',(0.489532925472927,-3.90414512413204,303.183165749349));
#6490=CARTESIAN_POINT('Ctrl Pts',(0.604735858539977,-3.88796695768318,303.189026713592));
#6491=CARTESIAN_POINT('Ctrl Pts',(0.718982318147405,-3.8667238621592,303.194887677835));
#6492=CARTESIAN_POINT('Ctrl Pts',(0.833240385486079,-3.84547860828262,303.200749237567));
#6493=CARTESIAN_POINT('Ctrl Pts',(0.946541381310529,-3.81916747760947,303.206610797299));
#6494=CARTESIAN_POINT('Ctrl Pts',(1.05841062355686,-3.78790917947381,303.212472357031));
#6495=CARTESIAN_POINT('Ctrl Pts',(1.17427186087416,-3.75553544540976,303.218543083439));
#6496=CARTESIAN_POINT('Ctrl Pts',(1.28859679338039,-3.71785500023293,303.224613809847));
#6497=CARTESIAN_POINT('Ctrl Pts',(1.4008764291635,-3.67505567715839,303.230684536255));
#6498=CARTESIAN_POINT('Ctrl Pts',(1.50944726630239,-3.63367009282895,303.236554735633));
#6499=CARTESIAN_POINT('Ctrl Pts',(1.61610543337687,-3.58749868482086,303.242424935011));
#6500=CARTESIAN_POINT('Ctrl Pts',(1.72041322114842,-3.53675944170617,303.24829513439));
#6501=CARTESIAN_POINT('Ctrl Pts',(1.83006576712664,-3.48342030656202,303.254466124313));
#6502=CARTESIAN_POINT('Ctrl Pts',(1.9371202206171,-3.42503307634299,303.260637114235));
#6503=CARTESIAN_POINT('Ctrl Pts',(2.04110095740479,-3.36190360981413,303.266808104158));
#6504=CARTESIAN_POINT('Ctrl Pts',(2.14508169419248,-3.29877414328527,303.272979094081));
#6505=CARTESIAN_POINT('Ctrl Pts',(2.24598832120404,-3.23090278988649,303.279150084004));
#6506=CARTESIAN_POINT('Ctrl Pts',(2.34338506086676,-3.15864456001407,303.285321073927));
#6507=CARTESIAN_POINT('Ctrl Pts',(2.43545879049995,-3.09033544880476,303.291154801624));
#6508=CARTESIAN_POINT('Ctrl Pts',(2.52470367385015,-3.01787791041709,303.29698852932));
#6509=CARTESIAN_POINT('Ctrl Pts',(2.61071910442475,-2.94153612212932,303.302822257017));
#6510=CARTESIAN_POINT('Ctrl Pts',(2.69662537708536,-2.86529121541622,303.308648581419));
#6511=CARTESIAN_POINT('Ctrl Pts',(2.77931003431553,-2.78517213482679,303.314474905821));
#6512=CARTESIAN_POINT('Ctrl Pts',(2.85840257146368,-2.70148546904288,303.320301230224));
#6513=CARTESIAN_POINT('Ctrl Pts',(2.93741660425641,-2.61788186757821,303.32612177163));
#6514=CARTESIAN_POINT('Ctrl Pts',(3.01284532077852,-2.53071802572051,303.331942313036));
#6515=CARTESIAN_POINT('Ctrl Pts',(3.08435294146453,-2.44033930683401,303.337762854442));
#6516=CARTESIAN_POINT('Ctrl Pts',(3.15581096158886,-2.35002327826189,303.343579358487));
#6517=CARTESIAN_POINT('Ctrl Pts',(3.22335303577711,-2.25649713550921,303.349395862531));
#6518=CARTESIAN_POINT('Ctrl Pts',(3.28668226398882,-2.16014089715956,303.355212366576));
#6519=CARTESIAN_POINT('Ctrl Pts',(3.34998888490214,-2.06381905610629,303.361026794242));
#6520=CARTESIAN_POINT('Ctrl Pts',(3.40908541899942,-1.96466947753097,303.366841221908));
#6521=CARTESIAN_POINT('Ctrl Pts',(3.46371747678195,-1.86310231630882,303.372655649574));
#6522=CARTESIAN_POINT('Ctrl Pts',(3.51834370030402,-1.76154600163531,303.378469456306));
#6523=CARTESIAN_POINT('Ctrl Pts',(3.56850619716011,-1.65757298708004,303.384283263039));
#6524=CARTESIAN_POINT('Ctrl Pts',(3.6139962460256,-1.55161855290302,303.390097069771));
#6525=CARTESIAN_POINT('Ctrl Pts',(3.65949281823104,-1.44564892470421,303.395911710212));
#6526=CARTESIAN_POINT('Ctrl Pts',(3.70031544598483,-1.33769769774431,303.401726350653));
#6527=CARTESIAN_POINT('Ctrl Pts',(3.73630362763664,-1.22821993230418,303.407540991094));
#6528=CARTESIAN_POINT('Ctrl Pts',(3.7723264008866,-1.11863693757223,303.413361220528));
#6529=CARTESIAN_POINT('Ctrl Pts',(3.80350531868779,-1.00752487358253,303.419181449962));
#6530=CARTESIAN_POINT('Ctrl Pts',(3.82972983561874,-0.895353777102462,303.425001679396));
#6531=CARTESIAN_POINT('Ctrl Pts',(3.85596803231133,-0.783124167671821,303.430824944896));
#6532=CARTESIAN_POINT('Ctrl Pts',(3.87724660440776,-0.669834837519033,303.436648210396));
#6533=CARTESIAN_POINT('Ctrl Pts',(3.89350651409067,-0.555964049857084,303.442471475895));
#6534=CARTESIAN_POINT('Ctrl Pts',(3.90979039676959,-0.4419253754116,303.448303326997));
#6535=CARTESIAN_POINT('Ctrl Pts',(3.9210408005791,-0.327303948478049,303.454135178099));
#6536=CARTESIAN_POINT('Ctrl Pts',(3.92725071313894,-0.212581363599228,303.459967029201));
#6537=CARTESIAN_POINT('Ctrl Pts',(3.93110874066186,-0.141307752948724,303.463590178778));
#6538=CARTESIAN_POINT('Ctrl Pts',(3.93302229924915,-0.06999509726729,303.467213328355));
#6539=CARTESIAN_POINT('Ctrl Pts',(3.93299980390471,0.00124196841145939,
303.470836477931));
#6540=CARTESIAN_POINT('',(3.93299876362378,-0.00311854674718142,304.720836477934));
#6541=CARTESIAN_POINT('Ctrl Pts',(3.9329998039045,0.00124196907699985,303.470836477965));
#6542=CARTESIAN_POINT('Ctrl Pts',(3.93297724349898,0.0726850284083443,303.474470104473));
#6543=CARTESIAN_POINT('Ctrl Pts',(3.93100814933993,0.144094335620644,303.47810373098));
#6544=CARTESIAN_POINT('Ctrl Pts',(3.92709733580092,0.215396181826265,303.481737357488));
#6545=CARTESIAN_POINT('Ctrl Pts',(3.92076713854636,0.330808166210949,303.487618888865));
#6546=CARTESIAN_POINT('Ctrl Pts',(3.90933474442503,0.446126778365148,303.493500420243));
#6547=CARTESIAN_POINT('Ctrl Pts',(3.89280348111204,0.560865453956625,303.49938195162));
#6548=CARTESIAN_POINT('Ctrl Pts',(3.87629310999173,0.675459122934113,303.505256049925));
#6549=CARTESIAN_POINT('Ctrl Pts',(3.85469674391957,0.789473908938345,303.51113014823));
#6550=CARTESIAN_POINT('Ctrl Pts',(3.82806966980477,0.902425400307849,303.517004246534));
#6551=CARTESIAN_POINT('Ctrl Pts',(3.80146919228528,1.01526406947644,303.522872477464));
#6552=CARTESIAN_POINT('Ctrl Pts',(3.76984809661393,1.12704115818054,303.528740708395));
#6553=CARTESIAN_POINT('Ctrl Pts',(3.73331311205916,1.23728016525246,303.534608939325));
#6554=CARTESIAN_POINT('Ctrl Pts',(3.69607585717752,1.34963817099025,303.540589968563));
#6555=CARTESIAN_POINT('Ctrl Pts',(3.65373391493134,1.46039792427612,303.546570997802));
#6556=CARTESIAN_POINT('Ctrl Pts',(3.60645441286487,1.56906837579739,303.55255202704));
#6557=CARTESIAN_POINT('Ctrl Pts',(3.56011760593738,1.67557207213044,303.55841380191));
#6558=CARTESIAN_POINT('Ctrl Pts',(3.50903848508585,1.78006861692458,303.564275576779));
#6559=CARTESIAN_POINT('Ctrl Pts',(3.45342355261713,1.88211444025843,303.570137351648));
#6560=CARTESIAN_POINT('Ctrl Pts',(3.39781631164719,1.98414615074,303.575998315839));
#6561=CARTESIAN_POINT('Ctrl Pts',(3.33767470358564,2.08372745229958,303.58185928003));
#6562=CARTESIAN_POINT('Ctrl Pts',(3.27325131613053,2.18043913500234,303.587720244221));
#6563=CARTESIAN_POINT('Ctrl Pts',(3.2088213830904,2.27716064386555,303.593581803901));
#6564=CARTESIAN_POINT('Ctrl Pts',(3.14010903413636,2.37101161154408,303.599443363581));
#6565=CARTESIAN_POINT('Ctrl Pts',(3.06740993956996,2.46160217391589,303.605304923261));
#6566=CARTESIAN_POINT('Ctrl Pts',(2.99211661446502,2.55542541483493,303.611375649743));
#6567=CARTESIAN_POINT('Ctrl Pts',(2.91254699512177,2.64575083865355,303.617446376226));
#6568=CARTESIAN_POINT('Ctrl Pts',(2.82907379728069,2.73218419026606,303.623517102708));
#6569=CARTESIAN_POINT('Ctrl Pts',(2.74835787122056,2.81576249082629,303.629387302036));
#6570=CARTESIAN_POINT('Ctrl Pts',(2.66399252506124,2.89570154048497,303.635257501364));
#6571=CARTESIAN_POINT('Ctrl Pts',(2.5763501968945,2.97168448240416,303.641127700692));
#6572=CARTESIAN_POINT('Ctrl Pts',(2.4842170501855,3.05156081250237,303.647298690751));
#6573=CARTESIAN_POINT('Ctrl Pts',(2.38846261490447,3.1270645437864,303.653469680811));
#6574=CARTESIAN_POINT('Ctrl Pts',(2.28955502976185,3.19787847888131,303.65964067087));
#6575=CARTESIAN_POINT('Ctrl Pts',(2.19064744461922,3.26869241397621,303.665811660929));
#6576=CARTESIAN_POINT('Ctrl Pts',(2.08858718539478,3.33481632871994,303.671982650989));
#6577=CARTESIAN_POINT('Ctrl Pts',(1.98387193327577,3.39598898001166,303.678153641048));
#6578=CARTESIAN_POINT('Ctrl Pts',(1.88406849122884,3.45429224562489,303.684035172499));
#6579=CARTESIAN_POINT('Ctrl Pts',(1.78153192407126,3.5082860844213,303.689916703951));
#6580=CARTESIAN_POINT('Ctrl Pts',(1.67667012221104,3.55770520157092,303.695798235402));
#6581=CARTESIAN_POINT('Ctrl Pts',(1.5719408445903,3.60706186289011,303.701672333779));
#6582=CARTESIAN_POINT('Ctrl Pts',(1.46489254604909,3.65185512709515,303.707546432157));
#6583=CARTESIAN_POINT('Ctrl Pts',(1.35595994737052,3.69186424738599,303.713420530535));
#6584=CARTESIAN_POINT('Ctrl Pts',(1.24713615661049,3.73183340434947,303.719288761537));
#6585=CARTESIAN_POINT('Ctrl Pts',(1.13643219418166,3.76702778222905,303.72515699254));
#6586=CARTESIAN_POINT('Ctrl Pts',(1.02430452134174,3.79727392316631,303.731025223543));
#6587=CARTESIAN_POINT('Ctrl Pts',(0.910021548103897,3.8281014506422,303.737006252754));
#6588=CARTESIAN_POINT('Ctrl Pts',(0.794259959271355,3.85378836150459,303.742987281965));
#6589=CARTESIAN_POINT('Ctrl Pts',(0.677521633415707,3.87420358735234,303.748968311176));
#6590=CARTESIAN_POINT('Ctrl Pts',(0.563110924342039,3.89421175903048,303.754830086116));
#6591=CARTESIAN_POINT('Ctrl Pts',(0.447762491066853,3.90915644642796,303.760691861056));
#6592=CARTESIAN_POINT('Ctrl Pts',(0.33196028223957,3.91896559962134,303.766553635996));
#6593=CARTESIAN_POINT('Ctrl Pts',(0.216174088777913,3.92877339621559,303.772414600256));
#6594=CARTESIAN_POINT('Ctrl Pts',(0.0999346547980537,3.93344703631303,303.778275564516));
#6595=CARTESIAN_POINT('Ctrl Pts',(-0.0162690097360618,3.9329663511556,303.784136528777));
#6596=CARTESIAN_POINT('Ctrl Pts',(-0.132484480848625,3.93248561715938,303.789998088526));
#6597=CARTESIAN_POINT('Ctrl Pts',(-0.248663763486618,3.92684951855352,303.795859648275));
#6598=CARTESIAN_POINT('Ctrl Pts',(-0.364318601620493,3.9160900087349,303.801721208024));
#6599=CARTESIAN_POINT('Ctrl Pts',(-0.484100520964409,3.90494655154738,303.807791934406));
#6600=CARTESIAN_POINT('Ctrl Pts',(-0.603319392770055,3.88830724208517,303.813862660788));
#6601=CARTESIAN_POINT('Ctrl Pts',(-0.721440848531566,3.86626591197114,303.81993338717));
#6602=CARTESIAN_POINT('Ctrl Pts',(-0.835660540602558,3.844952646551,303.825803586563));
#6603=CARTESIAN_POINT('Ctrl Pts',(-0.948853777669127,3.81858875686602,303.831673785957));
#6604=CARTESIAN_POINT('Ctrl Pts',(-1.06055093604124,3.78731048529983,303.837543985351));
#6605=CARTESIAN_POINT('Ctrl Pts',(-1.17797148469267,3.75442950729021,303.843714975227));
#6606=CARTESIAN_POINT('Ctrl Pts',(-1.29373807183921,3.71611734535315,303.849885965103));
#6607=CARTESIAN_POINT('Ctrl Pts',(-1.40732806354444,3.67258992014631,303.85605695498));
#6608=CARTESIAN_POINT('Ctrl Pts',(-1.52091805524966,3.62906249493948,303.862227944856));
#6609=CARTESIAN_POINT('Ctrl Pts',(-1.63233100231149,3.58032008001792,303.868398934732));
#6610=CARTESIAN_POINT('Ctrl Pts',(-1.74107469043908,3.52663407831213,303.874569924608));
#6611=CARTESIAN_POINT('Ctrl Pts',(-1.84471761548938,3.47546628782378,303.880451456237));
#6612=CARTESIAN_POINT('Ctrl Pts',(-1.9462699658564,3.41964332459861,303.886332987867));
#6613=CARTESIAN_POINT('Ctrl Pts',(-2.04528561596243,3.35935942541687,303.892214519496));
#6614=CARTESIAN_POINT('Ctrl Pts',(-2.14417613021617,3.29915171295002,303.898088618054));
#6615=CARTESIAN_POINT('Ctrl Pts',(-2.24053597150076,3.23449448940438,303.903962716611));
#6616=CARTESIAN_POINT('Ctrl Pts',(-2.33394140916372,3.16562892623107,303.909836815168));
#6617=CARTESIAN_POINT('Ctrl Pts',(-2.42725354831772,3.09683214978498,303.915705046351));
#6618=CARTESIAN_POINT('Ctrl Pts',(-2.51761682459389,3.02383563861823,303.921573277534));
#6619=CARTESIAN_POINT('Ctrl Pts',(-2.60463499393594,2.94692476123235,303.927441508718));
#6620=CARTESIAN_POINT('Ctrl Pts',(-2.69332580904191,2.86853551841737,303.933422537861));
#6621=CARTESIAN_POINT('Ctrl Pts',(-2.77854121904429,2.78608009789253,303.939403567005));
#6622=CARTESIAN_POINT('Ctrl Pts',(-2.85989533299847,2.69990512505413,303.945384596149));
#6623=CARTESIAN_POINT('Ctrl Pts',(-2.93962735064849,2.6154483702401,303.951246371271));
#6624=CARTESIAN_POINT('Ctrl Pts',(-3.01565032955656,2.52741932842187,303.957108146393));
#6625=CARTESIAN_POINT('Ctrl Pts',(-3.08763751042896,2.43618217795634,303.962969921515));
#6626=CARTESIAN_POINT('Ctrl Pts',(-3.15961473552719,2.3449576455216,303.968830885958));
#6627=CARTESIAN_POINT('Ctrl Pts',(-3.22755701756412,2.25052620999185,303.974691850401));
#6628=CARTESIAN_POINT('Ctrl Pts',(-3.2911781055904,2.15328485744047,303.980552814844));
#6629=CARTESIAN_POINT('Ctrl Pts',(-3.35480565767605,2.05603362492796,303.986414374775));
#6630=CARTESIAN_POINT('Ctrl Pts',(-3.41411091750535,1.95597225245877,303.992275934707));
#6631=CARTESIAN_POINT('Ctrl Pts',(-3.4688515474911,1.85352581354256,303.998137494638));
#6632=CARTESIAN_POINT('Ctrl Pts',(-3.5255455635182,1.74742363584846,304.004208220765));
#6633=CARTESIAN_POINT('Ctrl Pts',(-3.57734286543658,1.63876341196607,304.010278946893));
#6634=CARTESIAN_POINT('Ctrl Pts',(-3.62402734990921,1.52804278968556,304.01634967302));
#6635=CARTESIAN_POINT('Ctrl Pts',(-3.66916976535286,1.42097946049541,304.022219872595));
#6636=CARTESIAN_POINT('Ctrl Pts',(-3.70953171257518,1.31199011416512,304.02809007217));
#6637=CARTESIAN_POINT('Ctrl Pts',(-3.74496815269547,1.20154173264879,304.033960271744));
#6638=CARTESIAN_POINT('Ctrl Pts',(-3.78222036085575,1.0854339609526,304.040131261148));
#6639=CARTESIAN_POINT('Ctrl Pts',(-3.81402878617087,0.967714182480075,304.046302250552));
#6640=CARTESIAN_POINT('Ctrl Pts',(-3.84028567851689,0.848937516769068,304.052473239956));
#6641=CARTESIAN_POINT('Ctrl Pts',(-3.86654257086292,0.730160851058062,304.05864422936));
#6642=CARTESIAN_POINT('Ctrl Pts',(-3.88724791104503,0.610327823699778,304.064815218764));
#6643=CARTESIAN_POINT('Ctrl Pts',(-3.90235701070404,0.489998735721905,304.070986208168));
#6644=CARTESIAN_POINT('Ctrl Pts',(-3.91675739780014,0.375313844834309,304.076867739046));
#6645=CARTESIAN_POINT('Ctrl Pts',(-3.92612106289952,0.259808859864661,304.082749269924));
#6646=CARTESIAN_POINT('Ctrl Pts',(-3.93036431193775,0.143963104461184,304.088630800802));
#6647=CARTESIAN_POINT('Ctrl Pts',(-3.93460219836204,0.0282637548089151,
304.094504898607));
#6648=CARTESIAN_POINT('Ctrl Pts',(-3.93373252396109,-0.0877751007682438,
304.100378996412));
#6649=CARTESIAN_POINT('Ctrl Pts',(-3.92772310194429,-0.203666969470105,
304.106253094217));
#6650=CARTESIAN_POINT('Ctrl Pts',(-3.9217196824706,-0.319443078962975,304.112121324648));
#6651=CARTESIAN_POINT('Ctrl Pts',(-3.91058674917664,-0.43507208468703,304.11798955508));
#6652=CARTESIAN_POINT('Ctrl Pts',(-3.89434414314356,-0.550066082178732,
304.123857785511));
#6653=CARTESIAN_POINT('Ctrl Pts',(-3.87778932209959,-0.667270491725312,
304.129838814937));
#6654=CARTESIAN_POINT('Ctrl Pts',(-3.8559263462702,-0.783814794207662,304.135819844362));
#6655=CARTESIAN_POINT('Ctrl Pts',(-3.82883188209237,-0.899185975576223,
304.141800873788));
#6656=CARTESIAN_POINT('Ctrl Pts',(-3.80227765128556,-1.01225678437351,304.147662648163));
#6657=CARTESIAN_POINT('Ctrl Pts',(-3.77069871852815,-1.12420040153827,304.153524422539));
#6658=CARTESIAN_POINT('Ctrl Pts',(-3.73421897735477,-1.23454349018715,304.159386196914));
#6659=CARTESIAN_POINT('Ctrl Pts',(-3.69774428128287,-1.34487131852822,304.165247160614));
#6660=CARTESIAN_POINT('Ctrl Pts',(-3.65637025391693,-1.45359866766378,304.171108124313));
#6661=CARTESIAN_POINT('Ctrl Pts',(-3.61027048613083,-1.56026793114922,304.176969088013));
#6662=CARTESIAN_POINT('Ctrl Pts',(-3.56416603446161,-1.66694803257131,304.182830647205));
#6663=CARTESIAN_POINT('Ctrl Pts',(-3.51333505124083,-1.77156925463698,304.188692206397));
#6664=CARTESIAN_POINT('Ctrl Pts',(-3.4579987614115,-1.87369516359425,304.194553765589));
#6665=CARTESIAN_POINT('Ctrl Pts',(-3.4006878126345,-1.9794654050598,304.200624492767));
#6666=CARTESIAN_POINT('Ctrl Pts',(-3.33854423471032,-2.08255849745215,304.206695219946));
#6667=CARTESIAN_POINT('Ctrl Pts',(-3.27186427265409,-2.1825199154486,304.212765947124));
#6668=CARTESIAN_POINT('Ctrl Pts',(-3.20738688382552,-2.27917940680487,304.218636145976));
#6669=CARTESIAN_POINT('Ctrl Pts',(-3.13866836723035,-2.37291054688362,304.224506344829));
#6670=CARTESIAN_POINT('Ctrl Pts',(-3.06601852864048,-2.4633350121397,304.230376543681));
#6671=CARTESIAN_POINT('Ctrl Pts',(-2.98964606901135,-2.55839288090167,304.236547535022));
#6672=CARTESIAN_POINT('Ctrl Pts',(-2.90892907964158,-2.64979582975975,304.242718526363));
#6673=CARTESIAN_POINT('Ctrl Pts',(-2.8242714652856,-2.73714809434446,304.248889517705));
#6674=CARTESIAN_POINT('Ctrl Pts',(-2.73961385092963,-2.82450035892918,304.255060509046));
#6675=CARTESIAN_POINT('Ctrl Pts',(-2.65101603963972,-2.90780163364738,304.261231500387));
#6676=CARTESIAN_POINT('Ctrl Pts',(-2.55892100416771,-2.98670592700877,304.267402491728));
#6677=CARTESIAN_POINT('Ctrl Pts',(-2.47114582302524,-3.06190909737749,304.273284023561));
#6678=CARTESIAN_POINT('Ctrl Pts',(-2.37991126582219,-3.13336075402604,304.279165555394));
#6679=CARTESIAN_POINT('Ctrl Pts',(-2.28557123594851,-3.20072696826905,304.285047087227));
#6680=CARTESIAN_POINT('Ctrl Pts',(-2.19135043296191,-3.26800804512098,304.290921185983));
#6681=CARTESIAN_POINT('Ctrl Pts',(-2.09403229516527,-3.33121371109447,304.296795284739));
#6682=CARTESIAN_POINT('Ctrl Pts',(-1.99400508673938,-3.39004907251466,304.302669383495));
#6683=CARTESIAN_POINT('Ctrl Pts',(-1.89407779109888,-3.44882566587631,304.308537614871));
#6684=CARTESIAN_POINT('Ctrl Pts',(-1.79144716068113,-3.50324043079569,304.314405846248));
#6685=CARTESIAN_POINT('Ctrl Pts',(-1.68653130243143,-3.55304111514614,304.320274077624));
#6686=CARTESIAN_POINT('Ctrl Pts',(-1.57959877749203,-3.60379905593932,304.326255106694));
#6687=CARTESIAN_POINT('Ctrl Pts',(-1.4702926183206,-3.64976344900962,304.332236135763));
#6688=CARTESIAN_POINT('Ctrl Pts',(-1.35908319433564,-3.69071563126644,304.338217164832));
#6689=CARTESIAN_POINT('Ctrl Pts',(-1.25009113841468,-3.730851281454,304.344078940134));
#6690=CARTESIAN_POINT('Ctrl Pts',(-1.13927141557552,-3.76617259484159,304.349940715435));
#6691=CARTESIAN_POINT('Ctrl Pts',(-1.02708730308535,-3.79652218113379,304.355802490736));
#6692=CARTESIAN_POINT('Ctrl Pts',(-0.914918705681009,-3.82686757007196,
304.361663455353));
#6693=CARTESIAN_POINT('Ctrl Pts',(-0.801386491296358,-3.85224249181356,
304.367524419969));
#6694=CARTESIAN_POINT('Ctrl Pts',(-0.686968190209235,-3.87253969710327,
304.373385384586));
#6695=CARTESIAN_POINT('Ctrl Pts',(-0.572538264052435,-3.89283896461923,
304.379246944685));
#6696=CARTESIAN_POINT('Ctrl Pts',(-0.457222477702342,-3.90805941817867,
304.385108504785));
#6697=CARTESIAN_POINT('Ctrl Pts',(-0.341506935919518,-3.91814522608834,
304.390970064884));
#6698=CARTESIAN_POINT('Ctrl Pts',(-0.221662164081661,-3.92859093916294,
304.397040790751));
#6699=CARTESIAN_POINT('Ctrl Pts',(-0.101389048498594,-3.93352866481337,
304.403111516618));
#6700=CARTESIAN_POINT('Ctrl Pts',(0.0187698763244972,-3.93295521100136,
304.409182242485));
#6701=CARTESIAN_POINT('Ctrl Pts',(0.134959752648127,-3.9324006993195,304.415052442212));
#6702=CARTESIAN_POINT('Ctrl Pts',(0.251042448178382,-3.9266934278433,304.420922641939));
#6703=CARTESIAN_POINT('Ctrl Pts',(0.36653154990781,-3.91588350476903,304.426792841666));
#6704=CARTESIAN_POINT('Ctrl Pts',(0.487938316675192,-3.90451968091208,304.432963830603));
#6705=CARTESIAN_POINT('Ctrl Pts',(0.608688522367494,-3.88751650818532,304.43913481954));
#6706=CARTESIAN_POINT('Ctrl Pts',(0.728229356076895,-3.86499301486404,304.445305808477));
#6707=CARTESIAN_POINT('Ctrl Pts',(0.847770189786295,-3.84246952154276,304.451476797414));
#6708=CARTESIAN_POINT('Ctrl Pts',(0.966101160649947,-3.81442589648643,304.457647786351));
#6709=CARTESIAN_POINT('Ctrl Pts',(1.08268947065621,-3.78104119392135,304.463818775288));
#6710=CARTESIAN_POINT('Ctrl Pts',(1.19380909821671,-3.74922243168823,304.469700308285));
#6711=CARTESIAN_POINT('Ctrl Pts',(1.30370387732472,-3.71244979145023,304.475581841282));
#6712=CARTESIAN_POINT('Ctrl Pts',(1.41190014870259,-3.67083464216159,304.481463374279));
#6713=CARTESIAN_POINT('Ctrl Pts',(1.51995968195813,-3.62927208597345,304.487337474213));
#6714=CARTESIAN_POINT('Ctrl Pts',(1.62632459563915,-3.58287933893364,304.493211574146));
#6715=CARTESIAN_POINT('Ctrl Pts',(1.73053487570909,-3.53181795170059,304.499085674079));
#6716=CARTESIAN_POINT('Ctrl Pts',(1.83464106493965,-3.48080756733071,304.504953906645));
#6717=CARTESIAN_POINT('Ctrl Pts',(1.93659653404071,-3.4251379994445,304.510822139211));
#6718=CARTESIAN_POINT('Ctrl Pts',(2.03596041321068,-3.36501919694955,304.516690371777));
#6719=CARTESIAN_POINT('Ctrl Pts',(2.13723421230144,-3.30374482263658,304.522671400405));
#6720=CARTESIAN_POINT('Ctrl Pts',(2.23581535788513,-3.23784856044379,304.528652429033));
#6721=CARTESIAN_POINT('Ctrl Pts',(2.33126221796963,-3.16760247996293,304.534633457661));
#6722=CARTESIAN_POINT('Ctrl Pts',(2.42480602078419,-3.09875699363494,304.540495234173));
#6723=CARTESIAN_POINT('Ctrl Pts',(2.51533901948406,-3.02573379443896,304.546357010686));
#6724=CARTESIAN_POINT('Ctrl Pts',(2.6024746236808,-2.94883279164782,304.552218787198));
#6725=CARTESIAN_POINT('Ctrl Pts',(2.68959817709415,-2.871942424203,304.558079753031));
#6726=CARTESIAN_POINT('Ctrl Pts',(2.77332496173136,-2.79117559211882,304.563940718864));
#6727=CARTESIAN_POINT('Ctrl Pts',(2.85330237920067,-2.7068717244908,304.569801684697));
#6728=CARTESIAN_POINT('Ctrl Pts',(2.93328792255268,-2.62255929140316,304.575663246018));
#6729=CARTESIAN_POINT('Ctrl Pts',(3.00952305802561,-2.53470940712846,304.581524807338));
#6730=CARTESIAN_POINT('Ctrl Pts',(3.08169337310605,-2.44369698492965,304.587386368659));
#6731=CARTESIAN_POINT('Ctrl Pts',(3.15643900026495,-2.34943689241214,304.593457092841));
#6732=CARTESIAN_POINT('Ctrl Pts',(3.22682399347094,-2.25178471503604,304.599527817024));
#6733=CARTESIAN_POINT('Ctrl Pts',(3.29254678060488,-2.15119145998872,304.605598541206));
#6734=CARTESIAN_POINT('Ctrl Pts',(3.35609866596458,-2.05392091971635,304.611468742154));
#6735=CARTESIAN_POINT('Ctrl Pts',(3.41529131825077,-1.95390091967525,304.617338943101));
#6736=CARTESIAN_POINT('Ctrl Pts',(3.46989856609507,-1.85156499778198,304.623209144048));
#6737=CARTESIAN_POINT('Ctrl Pts',(3.52730384984093,-1.74398545723404,304.629380129848));
#6738=CARTESIAN_POINT('Ctrl Pts',(3.57964114955997,-1.6338468545087,304.635551115649));
#6739=CARTESIAN_POINT('Ctrl Pts',(3.62670522896991,-1.52167610948004,304.641722101449));
#6740=CARTESIAN_POINT('Ctrl Pts',(3.67376930837985,-1.40950536445138,304.647893087249));
#6741=CARTESIAN_POINT('Ctrl Pts',(3.7155600546515,-1.29530299081345,304.654064073049));
#6742=CARTESIAN_POINT('Ctrl Pts',(3.75193335141045,-1.17961227807018,304.660235058849));
#6743=CARTESIAN_POINT('Ctrl Pts',(3.79353038241778,-1.04730669694197,304.66729228793));
#6744=CARTESIAN_POINT('Ctrl Pts',(3.82815265954103,-0.912711690282679,304.674349517011));
#6745=CARTESIAN_POINT('Ctrl Pts',(3.85558531402917,-0.776499121855645,304.681406746093));
#6746=CARTESIAN_POINT('Ctrl Pts',(3.88272233690686,-0.641754466093948,304.688387922016));
#6747=CARTESIAN_POINT('Ctrl Pts',(3.90282382882847,-0.505426965597625,304.69536909794));
#6748=CARTESIAN_POINT('Ctrl Pts',(3.91572817428225,-0.368187269106653,304.702350273864));
#6749=CARTESIAN_POINT('Ctrl Pts',(3.92711844081548,-0.247050034554848,304.708512341887));
#6750=CARTESIAN_POINT('Ctrl Pts',(3.93290196110154,-0.12520239898195,304.714674409911));
#6751=CARTESIAN_POINT('Ctrl Pts',(3.93299876362378,-0.00311854674718404,
304.720836477935));
#6752=CARTESIAN_POINT('',(3.93299889167903,0.00295263467253422,305.970836478001));
#6753=CARTESIAN_POINT('Ctrl Pts',(3.93299876362426,-0.00311854614236361,
304.720836477965));
#6754=CARTESIAN_POINT('Ctrl Pts',(3.93309044288826,0.112504059879749,304.726672420641));
#6755=CARTESIAN_POINT('Ctrl Pts',(3.92807921482838,0.228206433372478,304.732508363318));
#6756=CARTESIAN_POINT('Ctrl Pts',(3.9179707306054,0.343503062751093,304.738344305994));
#6757=CARTESIAN_POINT('Ctrl Pts',(3.90786516887247,0.45876635842263,304.744178561426));
#6758=CARTESIAN_POINT('Ctrl Pts',(3.89266531672084,0.573623729284123,304.750012816858));
#6759=CARTESIAN_POINT('Ctrl Pts',(3.87242885259085,0.68759274401486,304.75584707229));
#6760=CARTESIAN_POINT('Ctrl Pts',(3.85219326980367,0.801556795142779,304.761681073628));
#6761=CARTESIAN_POINT('Ctrl Pts',(3.82692158407276,0.914632157675829,304.767515074965));
#6762=CARTESIAN_POINT('Ctrl Pts',(3.79672283545177,1.02634531750238,304.773349076302));
#6763=CARTESIAN_POINT('Ctrl Pts',(3.76651798635264,1.13808104461139,304.779184256172));
#6764=CARTESIAN_POINT('Ctrl Pts',(3.73138420430134,1.24845362061568,304.785019436041));
#6765=CARTESIAN_POINT('Ctrl Pts',(3.69148055445412,1.3570041695172,304.79085461591));
#6766=CARTESIAN_POINT('Ctrl Pts',(3.65153425451423,1.46567074016081,304.796696032577));
#6767=CARTESIAN_POINT('Ctrl Pts',(3.6068080497739,1.57251100390095,304.802537449243));
#6768=CARTESIAN_POINT('Ctrl Pts',(3.55750944186126,1.67708543940611,304.80837886591));
#6769=CARTESIAN_POINT('Ctrl Pts',(3.50818307740112,1.78171875335448,304.814223571463));
#6770=CARTESIAN_POINT('Ctrl Pts',(3.45427937636074,1.88408333071874,304.820068277017));
#6771=CARTESIAN_POINT('Ctrl Pts',(3.39605127137777,1.98376529916557,304.825912982571));
#6772=CARTESIAN_POINT('Ctrl Pts',(3.33772955186372,2.08360752837884,304.831767084779));
#6773=CARTESIAN_POINT('Ctrl Pts',(3.27506976679879,2.18075818474117,304.837621186986));
#6774=CARTESIAN_POINT('Ctrl Pts',(3.2083677514685,2.27483304251915,304.843475289194));
#6775=CARTESIAN_POINT('Ctrl Pts',(3.15832482018389,2.3454123439103,304.847867306933));
#6776=CARTESIAN_POINT('Ctrl Pts',(3.10600752986126,2.41426100054013,304.852259324671));
#6777=CARTESIAN_POINT('Ctrl Pts',(3.05155477118755,2.48123003335896,304.85665134241));
#6778=CARTESIAN_POINT('Ctrl Pts',(2.97863477273715,2.57091110532514,304.862532879626));
#6779=CARTESIAN_POINT('Ctrl Pts',(2.90164055801538,2.65751939625126,304.868414416843));
#6780=CARTESIAN_POINT('Ctrl Pts',(2.82086064578117,2.74066309806277,304.874295954059));
#6781=CARTESIAN_POINT('Ctrl Pts',(2.74018282350456,2.8237017225505,304.880170058167));
#6782=CARTESIAN_POINT('Ctrl Pts',(2.65572910359967,2.90328417339925,304.886044162274));
#6783=CARTESIAN_POINT('Ctrl Pts',(2.56782878935635,2.97905090734494,304.891918266382));
#6784=CARTESIAN_POINT('Ctrl Pts',(2.48001627536094,3.05474196081006,304.897786503072));
#6785=CARTESIAN_POINT('Ctrl Pts',(2.38876432557151,3.12662461182242,304.903654739763));
#6786=CARTESIAN_POINT('Ctrl Pts',(2.29443922717336,3.19437593792717,304.909522976454));
#6787=CARTESIAN_POINT('Ctrl Pts',(2.19830115435824,3.2634294775788,304.915504003517));
#6788=CARTESIAN_POINT('Ctrl Pts',(2.09897088014991,3.32819092729918,304.92148503058));
#6789=CARTESIAN_POINT('Ctrl Pts',(1.99687211471548,3.38836107247615,304.927466057643));
#6790=CARTESIAN_POINT('Ctrl Pts',(1.89680894080443,3.44733157692327,304.933327838132));
#6791=CARTESIAN_POINT('Ctrl Pts',(1.79408701740145,3.50189194113393,304.939189618621));
#6792=CARTESIAN_POINT('Ctrl Pts',(1.68913403009981,3.55180450311652,304.94505139911));
#6793=CARTESIAN_POINT('Ctrl Pts',(1.58419555880846,3.60171016171043,304.950912368859));
#6794=CARTESIAN_POINT('Ctrl Pts',(1.47702700908186,3.64696911966955,304.956773338607));
#6795=CARTESIAN_POINT('Ctrl Pts',(1.36807905218987,3.68739050101278,304.962634308355));
#6796=CARTESIAN_POINT('Ctrl Pts',(1.25912002717839,3.72781598879995,304.968495873525));
#6797=CARTESIAN_POINT('Ctrl Pts',(1.14838162173231,3.76340277975507,304.974357438694));
#6798=CARTESIAN_POINT('Ctrl Pts',(1.0363321338903,3.79400905484771,304.980219003864));
#6799=CARTESIAN_POINT('Ctrl Pts',(0.920284477662538,3.82570742811801,304.986289722372));
#6800=CARTESIAN_POINT('Ctrl Pts',(0.802830885987274,3.85206308735008,304.992360440881));
#6801=CARTESIAN_POINT('Ctrl Pts',(0.684504583500926,3.87297591977619,304.99843115939));
#6802=CARTESIAN_POINT('Ctrl Pts',(0.5700865613404,3.89319800796529,305.004301363987));
#6803=CARTESIAN_POINT('Ctrl Pts',(0.454852991523888,3.90833114846625,305.010171568585));
#6804=CARTESIAN_POINT('Ctrl Pts',(0.339291411066153,3.91833770091052,305.016041773183));
#6805=CARTESIAN_POINT('Ctrl Pts',(0.217808817780249,3.92885695770821,305.022212748647));
#6806=CARTESIAN_POINT('Ctrl Pts',(0.0959642402970337,3.93371035043805,305.028383724111));
#6807=CARTESIAN_POINT('Ctrl Pts',(-0.0256771418625223,3.93291618069668,
305.034554699576));
#6808=CARTESIAN_POINT('Ctrl Pts',(-0.147318524022069,3.93212201095531,305.04072567504));
#6809=CARTESIAN_POINT('Ctrl Pts',(-0.268756194151563,3.92568037682122,305.046896650504));
#6810=CARTESIAN_POINT('Ctrl Pts',(-0.389433934093832,3.91367221557659,305.053067625969));
#6811=CARTESIAN_POINT('Ctrl Pts',(-0.50445161464586,3.90222726429798,305.058949168704));
#6812=CARTESIAN_POINT('Ctrl Pts',(-0.619149616709469,3.88568926349385,305.064830711439));
#6813=CARTESIAN_POINT('Ctrl Pts',(-0.733042001163635,3.86408312857397,305.070712254175));
#6814=CARTESIAN_POINT('Ctrl Pts',(-0.846790450691664,3.8425042990569,305.076586363933));
#6815=CARTESIAN_POINT('Ctrl Pts',(-0.959734906402532,3.81587015009463,305.082460473692));
#6816=CARTESIAN_POINT('Ctrl Pts',(-1.07139388540056,3.78425740962825,305.088334583451));
#6817=CARTESIAN_POINT('Ctrl Pts',(-1.18294133498977,3.7526762452186,305.094202825916));
#6818=CARTESIAN_POINT('Ctrl Pts',(-1.29320546803174,3.71612649307839,305.100071068381));
#6819=CARTESIAN_POINT('Ctrl Pts',(-1.40171498704683,3.67473592181647,305.105939310847));
#6820=CARTESIAN_POINT('Ctrl Pts',(-1.51230996396627,3.6325498600318,305.111920335792));
#6821=CARTESIAN_POINT('Ctrl Pts',(-1.62108175866984,3.58533506478871,305.117901360737));
#6822=CARTESIAN_POINT('Ctrl Pts',(-1.72754722374054,3.533280287459,305.123882385682));
#6823=CARTESIAN_POINT('Ctrl Pts',(-1.83189018077566,3.48226328029353,305.12974417221));
#6824=CARTESIAN_POINT('Ctrl Pts',(-1.93401752879696,3.42659767395453,305.135605958738));
#6825=CARTESIAN_POINT('Ctrl Pts',(-2.03349529634568,3.36650945041597,305.141467745267));
#6826=CARTESIAN_POINT('Ctrl Pts',(-2.13295930665367,3.30642953675584,305.147328721141));
#6827=CARTESIAN_POINT('Ctrl Pts',(-2.22977411279647,3.24192843509472,305.153189697016));
#6828=CARTESIAN_POINT('Ctrl Pts',(-2.32353212423129,3.17327708649358,305.159050672891));
#6829=CARTESIAN_POINT('Ctrl Pts',(-2.4172996618925,3.10461876261345,305.164912244266));
#6830=CARTESIAN_POINT('Ctrl Pts',(-2.50800945517101,3.03180959680641,305.170773815642));
#6831=CARTESIAN_POINT('Ctrl Pts',(-2.59528514209377,2.95516226817197,305.176635387017));
#6832=CARTESIAN_POINT('Ctrl Pts',(-2.68567479525653,2.87578018943508,305.182706097227));
#6833=CARTESIAN_POINT('Ctrl Pts',(-2.77238034983704,2.7922812563357,305.188776807436));
#6834=CARTESIAN_POINT('Ctrl Pts',(-2.85502448088432,2.7050553069302,305.194847517645));
#6835=CARTESIAN_POINT('Ctrl Pts',(-2.93493909807435,2.62071019654613,305.200717728588));
#6836=CARTESIAN_POINT('Ctrl Pts',(-3.01105610450854,2.53288072603806,305.206587939531));
#6837=CARTESIAN_POINT('Ctrl Pts',(-3.08307547968066,2.44195302710594,305.212458150474));
#6838=CARTESIAN_POINT('Ctrl Pts',(-3.15878462819027,2.34636682345398,305.218629110317));
#6839=CARTESIAN_POINT('Ctrl Pts',(-3.22996484790023,2.24735695006518,305.224800070159));
#6840=CARTESIAN_POINT('Ctrl Pts',(-3.29632003011824,2.14540515032506,305.230971030002));
#6841=CARTESIAN_POINT('Ctrl Pts',(-3.36267521233624,2.04345335058495,305.237141989844));
#6842=CARTESIAN_POINT('Ctrl Pts',(-3.42420515423831,1.93856010973155,305.243312949687));
#6843=CARTESIAN_POINT('Ctrl Pts',(-3.48067095548873,1.83123420119251,305.249483909529));
#6844=CARTESIAN_POINT('Ctrl Pts',(-3.53448793321464,1.72894297532923,305.255365388248));
#6845=CARTESIAN_POINT('Ctrl Pts',(-3.58387854436078,1.62411255661549,305.261246866967));
#6846=CARTESIAN_POINT('Ctrl Pts',(-3.62859585370637,1.51716219649217,305.267128345686));
#6847=CARTESIAN_POINT('Ctrl Pts',(-3.67325664837305,1.41034700249021,305.273002391267));
#6848=CARTESIAN_POINT('Ctrl Pts',(-3.71325573030816,1.30141757231233,305.278876436849));
#6849=CARTESIAN_POINT('Ctrl Pts',(-3.7483918586729,1.19081798518276,305.284750482431));
#6850=CARTESIAN_POINT('Ctrl Pts',(-3.78349289082057,1.08032887200973,305.29061866064));
#6851=CARTESIAN_POINT('Ctrl Pts',(-3.81374050809356,0.968173310775371,305.296486838848));
#6852=CARTESIAN_POINT('Ctrl Pts',(-3.83898167650097,0.854815001909668,305.302355017057));
#6853=CARTESIAN_POINT('Ctrl Pts',(-3.86470834323288,0.739276315807282,305.308336066058));
#6854=CARTESIAN_POINT('Ctrl Pts',(-3.88523380992108,0.622488536375575,305.31431711506));
#6855=CARTESIAN_POINT('Ctrl Pts',(-3.90044940169039,0.504958874417568,305.320298164061));
#6856=CARTESIAN_POINT('Ctrl Pts',(-3.91536143074368,0.389774019282671,305.326159886552));
#6857=CARTESIAN_POINT('Ctrl Pts',(-3.92517343842528,0.273877036136198,305.332021609042));
#6858=CARTESIAN_POINT('Ctrl Pts',(-3.92983491896867,0.157754586793943,305.337883331532));
#6859=CARTESIAN_POINT('Ctrl Pts',(-3.93449575500278,0.0416481928647091,
305.343744243564));
#6860=CARTESIAN_POINT('Ctrl Pts',(-3.93400746358965,-0.0746831938899506,
305.349605155597));
#6861=CARTESIAN_POINT('Ctrl Pts',(-3.9283715936104,-0.190750157312963,305.355466067629));
#6862=CARTESIAN_POINT('Ctrl Pts',(-3.92273515073891,-0.306828919067288,
305.361327575429));
#6863=CARTESIAN_POINT('Ctrl Pts',(-3.91195010908134,-0.4226427927254,305.367189083229));
#6864=CARTESIAN_POINT('Ctrl Pts',(-3.89607005488542,-0.537705428115716,
305.37305059103));
#6865=CARTESIAN_POINT('Ctrl Pts',(-3.87962298375207,-0.65687651693619,305.379121391201));
#6866=CARTESIAN_POINT('Ctrl Pts',(-3.85771031474405,-0.77524124443046,305.385192191373));
#6867=CARTESIAN_POINT('Ctrl Pts',(-3.83044950539371,-0.892269906826998,
305.391262991545));
#6868=CARTESIAN_POINT('Ctrl Pts',(-3.80408971790723,-1.00543054820616,305.397133140165));
#6869=CARTESIAN_POINT('Ctrl Pts',(-3.77272990870503,-1.11734166185968,305.403003288786));
#6870=CARTESIAN_POINT('Ctrl Pts',(-3.73652702454398,-1.22754013981316,305.408873437406));
#6871=CARTESIAN_POINT('Ctrl Pts',(-3.69846792719186,-1.34338877170195,305.415044563353));
#6872=CARTESIAN_POINT('Ctrl Pts',(-3.65505614719676,-1.4573439958255,305.421215689301));
#6873=CARTESIAN_POINT('Ctrl Pts',(-3.60653060591148,-1.56889323684684,305.427386815248));
#6874=CARTESIAN_POINT('Ctrl Pts',(-3.5580050646262,-1.68044247786819,305.433557941195));
#6875=CARTESIAN_POINT('Ctrl Pts',(-3.50436605532843,-1.78958529909671,305.439729067143));
#6876=CARTESIAN_POINT('Ctrl Pts',(-3.44590658322787,-1.89584198172391,305.44590019309));
#6877=CARTESIAN_POINT('Ctrl Pts',(-3.39018977251935,-1.99711356799945,305.451781796942));
#6878=CARTESIAN_POINT('Ctrl Pts',(-3.32991504359332,-2.09609001318154,305.457663400793));
#6879=CARTESIAN_POINT('Ctrl Pts',(-3.2652962449239,-2.19233424296704,305.463545004645));
#6880=CARTESIAN_POINT('Ctrl Pts',(-3.20075911357354,-2.28845683619503,305.469419175136));
#6881=CARTESIAN_POINT('Ctrl Pts',(-3.13188905916723,-2.38185374270415,305.475293345627));
#6882=CARTESIAN_POINT('Ctrl Pts',(-3.05894582471176,-2.47211234402453,305.481167516118));
#6883=CARTESIAN_POINT('Ctrl Pts',(-2.98607545371347,-2.56228078545853,305.487035818863));
#6884=CARTESIAN_POINT('Ctrl Pts',(-2.90914025381092,-2.64931683929501,305.492904121609));
#6885=CARTESIAN_POINT('Ctrl Pts',(-2.82844290172965,-2.73283730793752,305.498772424354));
#6886=CARTESIAN_POINT('Ctrl Pts',(-2.74619577515903,-2.81796176838771,305.504753426533));
#6887=CARTESIAN_POINT('Ctrl Pts',(-2.6600407439559,-2.89943385647308,305.510734428712));
#6888=CARTESIAN_POINT('Ctrl Pts',(-2.57034120387822,-2.9768834534872,305.516715430891));
#6889=CARTESIAN_POINT('Ctrl Pts',(-2.48242870808692,-3.05279005641566,305.522577276207));
#6890=CARTESIAN_POINT('Ctrl Pts',(-2.39111195352829,-3.12483268079289,305.528439121524));
#6891=CARTESIAN_POINT('Ctrl Pts',(-2.29676926524284,-3.19270104178826,305.53430096684));
#6892=CARTESIAN_POINT('Ctrl Pts',(-2.20243963450449,-3.26056000942909,305.540162000845));
#6893=CARTESIAN_POINT('Ctrl Pts',(-2.10508523711594,-3.32424562222826,305.54602303485));
#6894=CARTESIAN_POINT('Ctrl Pts',(-2.00511537627614,-3.38348951938986,305.551884068855));
#6895=CARTESIAN_POINT('Ctrl Pts',(-1.90513537045563,-3.44273942864538,305.557745697639));
#6896=CARTESIAN_POINT('Ctrl Pts',(-1.80253972781519,-3.49754651627313,305.563607326424));
#6897=CARTESIAN_POINT('Ctrl Pts',(-1.69776386313948,-3.54768753768109,305.569468955209));
#6898=CARTESIAN_POINT('Ctrl Pts',(-1.58925218591523,-3.5996163511302,305.575539581996));
#6899=CARTESIAN_POINT('Ctrl Pts',(-1.4784023406849,-3.64653993997509,305.581610208782));
#6900=CARTESIAN_POINT('Ctrl Pts',(-1.36572103949845,-3.68826450275347,305.587680835569));
#6901=CARTESIAN_POINT('Ctrl Pts',(-1.25675877934779,-3.72861194830352,305.593551101605));
#6902=CARTESIAN_POINT('Ctrl Pts',(-1.14608446715669,-3.76409807133267,305.599421367641));
#6903=CARTESIAN_POINT('Ctrl Pts',(-1.03417106821957,-3.79459868782689,305.605291633676));
#6904=CARTESIAN_POINT('Ctrl Pts',(-0.916528017715103,-3.82666085018391,
305.611462440839));
#6905=CARTESIAN_POINT('Ctrl Pts',(-0.797516163788637,-3.85321339208828,
305.617633248001));
#6906=CARTESIAN_POINT('Ctrl Pts',(-0.677694801964336,-3.87417329960735,
305.623804055163));
#6907=CARTESIAN_POINT('Ctrl Pts',(-0.557873440140036,-3.89513320712642,
305.629974862325));
#6908=CARTESIAN_POINT('Ctrl Pts',(-0.437243096222677,-3.91050048438429,
305.636145669488));
#6909=CARTESIAN_POINT('Ctrl Pts',(-0.31636544559735,-3.92025533668816,305.64231647665));
#6910=CARTESIAN_POINT('Ctrl Pts',(-0.201152959526222,-3.92955300899872,
305.648198077017));
#6911=CARTESIAN_POINT('Ctrl Pts',(-0.0853447024464972,-3.93378238806566,
305.654079677383));
#6912=CARTESIAN_POINT('Ctrl Pts',(0.0305767478697531,-3.93288114014264,
305.65996127775));
#6913=CARTESIAN_POINT('Ctrl Pts',(0.146351717495847,-3.93198103105474,305.665835446007));
#6914=CARTESIAN_POINT('Ctrl Pts',(0.262239187654835,-3.92596319218012,305.671709614265));
#6915=CARTESIAN_POINT('Ctrl Pts',(0.377751705307836,-3.91481706458131,305.677583782522));
#6916=CARTESIAN_POINT('Ctrl Pts',(0.493148861045902,-3.90368206857802,305.68345208427));
#6917=CARTESIAN_POINT('Ctrl Pts',(0.6081714015849,-3.88742901138595,305.689320386017));
#6918=CARTESIAN_POINT('Ctrl Pts',(0.722332773385868,-3.86609937333389,305.695188687765));
#6919=CARTESIAN_POINT('Ctrl Pts',(0.838686624754658,-3.84436009763574,305.701169690784));
#6920=CARTESIAN_POINT('Ctrl Pts',(0.954145453613655,-3.81734723856571,305.707150693802));
#6921=CARTESIAN_POINT('Ctrl Pts',(1.06820016894353,-3.78516015500917,305.713131696821));
#6922=CARTESIAN_POINT('Ctrl Pts',(1.17998264550101,-3.75361431402656,305.718993544161));
#6923=CARTESIAN_POINT('Ctrl Pts',(1.29041602344907,-3.71709862327207,305.724855391501));
#6924=CARTESIAN_POINT('Ctrl Pts',(1.39903292108217,-3.67575786549227,305.730717238842));
#6925=CARTESIAN_POINT('Ctrl Pts',(1.50763480623193,-3.63442282162486,305.736578275987));
#6926=CARTESIAN_POINT('Ctrl Pts',(1.61442032559998,-3.5882641834342,305.742439313132));
#6927=CARTESIAN_POINT('Ctrl Pts',(1.71894001818385,-3.53747568385793,305.748300350277));
#6928=CARTESIAN_POINT('Ctrl Pts',(1.82347033721226,-3.48668202065018,305.75416198331));
#6929=CARTESIAN_POINT('Ctrl Pts',(1.92573400112539,-3.43125774028996,305.760023616343));
#6930=CARTESIAN_POINT('Ctrl Pts',(2.02530481479121,-3.37144322318848,305.765885249376));
#6931=CARTESIAN_POINT('Ctrl Pts',(2.12842576372008,-3.30949605678359,305.771955875278));
#6932=CARTESIAN_POINT('Ctrl Pts',(2.22865784474234,-3.24283999139748,305.778026501181));
#6933=CARTESIAN_POINT('Ctrl Pts',(2.3255601554877,-3.17179112855939,305.784097127084));
#6934=CARTESIAN_POINT('Ctrl Pts',(2.41926433453014,-3.10308713880998,305.789967400065));
#6935=CARTESIAN_POINT('Ctrl Pts',(2.50985477757929,-3.0302760439035,305.795837673045));
#6936=CARTESIAN_POINT('Ctrl Pts',(2.59696727228205,-2.9536841379362,305.801707946025));
#6937=CARTESIAN_POINT('Ctrl Pts',(2.68853950240764,-2.87317109944583,305.807878748389));
#6938=CARTESIAN_POINT('Ctrl Pts',(2.77626787070472,-2.78848025421607,305.814049550754));
#6939=CARTESIAN_POINT('Ctrl Pts',(2.85977496296949,-2.70003262224234,305.820220353118));
#6940=CARTESIAN_POINT('Ctrl Pts',(2.94328205523427,-2.6115849902686,305.826391155482));
#6941=CARTESIAN_POINT('Ctrl Pts',(3.02256758523281,-2.51938101262983,305.832561957846));
#6942=CARTESIAN_POINT('Ctrl Pts',(3.09730558680027,-2.42387852459149,305.83873276021));
#6943=CARTESIAN_POINT('Ctrl Pts',(3.16841691842985,-2.33301030553409,305.844604123695));
#6944=CARTESIAN_POINT('Ctrl Pts',(3.23564594367985,-2.23885685477851,305.85047548718));
#6945=CARTESIAN_POINT('Ctrl Pts',(3.29867404781631,-2.14178395882105,305.856346850665));
#6946=CARTESIAN_POINT('Ctrl Pts',(3.36162482580041,-2.04483015693512,305.862211010856));
#6947=CARTESIAN_POINT('Ctrl Pts',(3.42038470572425,-1.9449643728561,305.868075171047));
#6948=CARTESIAN_POINT('Ctrl Pts',(3.47467530420241,-1.84258528442129,305.873939331238));
#6949=CARTESIAN_POINT('Ctrl Pts',(3.52891241516199,-1.74030706065825,305.879797714013));
#6950=CARTESIAN_POINT('Ctrl Pts',(3.57868880782915,-1.63552081851714,305.885656096788));
#6951=CARTESIAN_POINT('Ctrl Pts',(3.62376980907873,-1.52865345020038,305.891514479563));
#6952=CARTESIAN_POINT('Ctrl Pts',(3.66881728756418,-1.42186554971887,305.897368505976));
#6953=CARTESIAN_POINT('Ctrl Pts',(3.70917615958446,-1.31299998020192,305.903222532388));
#6954=CARTESIAN_POINT('Ctrl Pts',(3.74465838158372,-1.20250680049421,305.909076558801));
#6955=CARTESIAN_POINT('Ctrl Pts',(3.78012564973577,-1.09206018771589,305.914928118057));
#6956=CARTESIAN_POINT('Ctrl Pts',(3.81072022758069,-0.979987720829308,305.920779677312));
#6957=CARTESIAN_POINT('Ctrl Pts',(3.83630298977896,-0.866757388554042,305.926631236567));
#6958=CARTESIAN_POINT('Ctrl Pts',(3.86187930737916,-0.753555580328454,305.932481321746));
#6959=CARTESIAN_POINT('Ctrl Pts',(3.88244623339217,-0.639196890247835,305.938331406925));
#6960=CARTESIAN_POINT('Ctrl Pts',(3.89791529686582,-0.524161557594061,305.944181492104));
#6961=CARTESIAN_POINT('Ctrl Pts',(3.91338784716017,-0.409100295278861,305.950032895928));
#6962=CARTESIAN_POINT('Ctrl Pts',(3.92376018391224,-0.293362494978405,305.955884299752));
#6963=CARTESIAN_POINT('Ctrl Pts',(3.92899551174811,-0.177435252030728,305.961735703575));
#6964=CARTESIAN_POINT('Ctrl Pts',(3.93170970586436,-0.117334136955256,305.964769295039));
#6965=CARTESIAN_POINT('Ctrl Pts',(3.93304403689269,-0.0571821728465312,
305.967802886502));
#6966=CARTESIAN_POINT('Ctrl Pts',(3.93299889167956,0.00295263396733381,
305.970836477965));
#6967=CARTESIAN_POINT('',(1.74869860048799,-3.52285994678348,306.999909416517));
#6968=CARTESIAN_POINT('Ctrl Pts',(3.93299889167903,0.0029526346725509,305.970836478001));
#6969=CARTESIAN_POINT('Ctrl Pts',(3.93289712360706,0.138510791597115,305.977674914663));
#6970=CARTESIAN_POINT('Ctrl Pts',(3.92578303440299,0.273785134511518,305.984513351326));
#6971=CARTESIAN_POINT('Ctrl Pts',(3.91176797889345,0.408117972287244,305.991351787988));
#6972=CARTESIAN_POINT('Ctrl Pts',(3.89766593117476,0.543284621267804,305.998232671198));
#6973=CARTESIAN_POINT('Ctrl Pts',(3.87657709023588,0.677497944107449,306.005113554408));
#6974=CARTESIAN_POINT('Ctrl Pts',(3.84866405746424,0.810107383488669,306.011994437617));
#6975=CARTESIAN_POINT('Ctrl Pts',(3.82056658327726,0.943593068489225,306.018920787754));
#6976=CARTESIAN_POINT('Ctrl Pts',(3.78555451165409,1.07545351169804,306.025847137892));
#6977=CARTESIAN_POINT('Ctrl Pts',(3.74384194762071,1.20504625273704,306.032773488029));
#6978=CARTESIAN_POINT('Ctrl Pts',(3.73907317719976,1.21986188549801,306.033565339942));
#6979=CARTESIAN_POINT('Ctrl Pts',(3.73421688150865,1.23464790254472,306.034357191856));
#6980=CARTESIAN_POINT('Ctrl Pts',(3.72927341967739,1.24940336212437,306.03514904377));
#6981=CARTESIAN_POINT('Ctrl Pts',(3.69255031001881,1.35901609480088,306.041031412373));
#6982=CARTESIAN_POINT('Ctrl Pts',(3.65093134138518,1.46718473829337,306.046913780975));
#6983=CARTESIAN_POINT('Ctrl Pts',(3.60454887307558,1.57344094951465,306.052796149578));
#6984=CARTESIAN_POINT('Ctrl Pts',(3.55822503132245,1.67956285490887,306.058671082978));
#6985=CARTESIAN_POINT('Ctrl Pts',(3.50714982803897,1.78377676160783,306.064546016379));
#6986=CARTESIAN_POINT('Ctrl Pts',(3.45150514742175,1.88563019102929,306.07042094978));
#6987=CARTESIAN_POINT('Ctrl Pts',(3.39591606944379,1.9873818439749,306.076290012685));
#6988=CARTESIAN_POINT('Ctrl Pts',(3.33576679346814,2.08677735246546,306.082159075591));
#6989=CARTESIAN_POINT('Ctrl Pts',(3.27128670288703,2.18338551509221,306.088028138497));
#6990=CARTESIAN_POINT('Ctrl Pts',(3.20557994039594,2.2818315554003,306.094008854699));
#6991=CARTESIAN_POINT('Ctrl Pts',(3.13537607156481,2.37738271336941,306.0999895709));
#6992=CARTESIAN_POINT('Ctrl Pts',(3.06096640292507,2.46961002592797,306.105970287102));
#6993=CARTESIAN_POINT('Ctrl Pts',(2.98802636484449,2.56001579997679,306.111832880975));
#6994=CARTESIAN_POINT('Ctrl Pts',(2.91104540726783,2.64722748579805,306.117695474848));
#6995=CARTESIAN_POINT('Ctrl Pts',(2.83034036601032,2.73087209743199,306.123558068721));
#6996=CARTESIAN_POINT('Ctrl Pts',(2.74964657103553,2.81450505315279,306.12941984564));
#6997=CARTESIAN_POINT('Ctrl Pts',(2.66523001020445,2.8945716270458,306.135281622558));
#6998=CARTESIAN_POINT('Ctrl Pts',(2.57744549293198,2.97073454400837,306.141143399476));
#6999=CARTESIAN_POINT('Ctrl Pts',(2.48965216515674,3.04690510507051,306.147005764712));
#7000=CARTESIAN_POINT('Ctrl Pts',(2.39849051993202,3.11917096056775,306.152868129949));
#7001=CARTESIAN_POINT('Ctrl Pts',(2.30434912397615,3.18723455597958,306.158730495185));
#7002=CARTESIAN_POINT('Ctrl Pts',(2.20688031948798,3.25770384535646,306.16480006453));
#7003=CARTESIAN_POINT('Ctrl Pts',(2.10621761237537,3.32366803967249,306.170869633876));
#7004=CARTESIAN_POINT('Ctrl Pts',(2.00282457289611,3.38484604231913,306.176939203221));
#7005=CARTESIAN_POINT('Ctrl Pts',(1.9028144410297,3.44402236736799,306.18281018287));
#7006=CARTESIAN_POINT('Ctrl Pts',(1.8002502481252,3.49872065916166,306.188681162519));
#7007=CARTESIAN_POINT('Ctrl Pts',(1.69557521418941,3.54873409725588,306.194552142168));
#7008=CARTESIAN_POINT('Ctrl Pts',(1.58558912882462,3.60128514085041,306.200721006362));
#7009=CARTESIAN_POINT('Ctrl Pts',(1.47327286760583,3.64866324838575,306.206889870556));
#7010=CARTESIAN_POINT('Ctrl Pts',(1.35916126896394,3.69068687982987,306.21305873475));
#7011=CARTESIAN_POINT('Ctrl Pts',(1.24504967032204,3.73271051127399,306.219227598944));
#7012=CARTESIAN_POINT('Ctrl Pts',(1.12914325102822,3.76937957672615,306.225396463137));
#7013=CARTESIAN_POINT('Ctrl Pts',(1.01199048658119,3.80057420070562,306.231565327331));
#7014=CARTESIAN_POINT('Ctrl Pts',(0.900289528946039,3.83031715545383,306.237447118011));
#7015=CARTESIAN_POINT('Ctrl Pts',(0.787096575424546,3.85517935422195,306.24332890869));
#7016=CARTESIAN_POINT('Ctrl Pts',(0.672875349500288,3.87501325985278,306.249210699369));
#7017=CARTESIAN_POINT('Ctrl Pts',(0.558798290772029,3.89482213162027,306.255085066198));
#7018=CARTESIAN_POINT('Ctrl Pts',(0.443695943088427,3.90961526284367,306.260959433027));
#7019=CARTESIAN_POINT('Ctrl Pts',(0.328046073160477,3.91929518840875,306.266833799856));
#7020=CARTESIAN_POINT('Ctrl Pts',(0.212511542925758,3.92896546001014,306.272702308074));
#7021=CARTESIAN_POINT('Ctrl Pts',(0.0964309847241987,3.93353263604942,306.278570816291));
#7022=CARTESIAN_POINT('Ctrl Pts',(-0.0197094256938501,3.93295061481057,
306.284439324509));
#7023=CARTESIAN_POINT('Ctrl Pts',(-0.138074685903231,3.93235744405169,306.290420253108));
#7024=CARTESIAN_POINT('Ctrl Pts',(-0.256501686965844,3.9264156878078,306.296401181707));
#7025=CARTESIAN_POINT('Ctrl Pts',(-0.374471814396688,3.91513216382569,306.302382110306));
#7026=CARTESIAN_POINT('Ctrl Pts',(-0.490097563316956,3.90407287331458,306.308244182032));
#7027=CARTESIAN_POINT('Ctrl Pts',(-0.605284001584659,3.88788220695453,306.314106253758));
#7028=CARTESIAN_POINT('Ctrl Pts',(-0.719545364824838,3.86661912631165,306.319968325485));
#7029=CARTESIAN_POINT('Ctrl Pts',(-0.83379105761463,3.84535896180807,306.325829593253));
#7030=CARTESIAN_POINT('Ctrl Pts',(-0.94711152298397,3.81902784179355,306.331690861021));
#7031=CARTESIAN_POINT('Ctrl Pts',(-1.05902988500892,3.78773609200245,306.337552128789));
#7032=CARTESIAN_POINT('Ctrl Pts',(-1.1709597387215,3.75644112919958,306.343413998388));
#7033=CARTESIAN_POINT('Ctrl Pts',(-1.28148680634442,3.72018463492664,306.349275867987));
#7034=CARTESIAN_POINT('Ctrl Pts',(-1.39014877040593,3.67912698831379,306.355137737585));
#7035=CARTESIAN_POINT('Ctrl Pts',(-1.50267484833663,3.63660929610832,306.361208060361));
#7036=CARTESIAN_POINT('Ctrl Pts',(-1.61320025723283,3.58894279412773,306.367278383136));
#7037=CARTESIAN_POINT('Ctrl Pts',(-1.72123481044774,3.5363596716543,306.373348705912));
#7038=CARTESIAN_POINT('Ctrl Pts',(-1.82571347588474,3.48550728880967,306.37921922792));
#7039=CARTESIAN_POINT('Ctrl Pts',(-1.92786233770892,3.43005710205278,306.385089749929));
#7040=CARTESIAN_POINT('Ctrl Pts',(-2.02726471187947,3.37026509164609,306.390960271938));
#7041=CARTESIAN_POINT('Ctrl Pts',(-2.13174176353459,3.30742058705604,306.397130495097));
#7042=CARTESIAN_POINT('Ctrl Pts',(-2.23318405934418,3.23977953541925,306.403300718256));
#7043=CARTESIAN_POINT('Ctrl Pts',(-2.33114517600648,3.16768861607035,306.409470941414));
#7044=CARTESIAN_POINT('Ctrl Pts',(-2.4291062926688,3.09559769672145,306.415641164573));
#7045=CARTESIAN_POINT('Ctrl Pts',(-2.52358587003434,3.01905729220659,306.421811387732));
#7046=CARTESIAN_POINT('Ctrl Pts',(-2.61418150222925,2.93845947281946,306.427981610891));
#7047=CARTESIAN_POINT('Ctrl Pts',(-2.70047380925804,2.86169007888839,306.433858746227));
#7048=CARTESIAN_POINT('Ctrl Pts',(-2.78352190916399,2.78099146830398,306.439735881563));
#7049=CARTESIAN_POINT('Ctrl Pts',(-2.86294739944237,2.69666853506807,306.445613016899));
#7050=CARTESIAN_POINT('Ctrl Pts',(-2.94227227116643,2.61245242461171,306.451482706906));
#7051=CARTESIAN_POINT('Ctrl Pts',(-3.01798337984358,2.5246214204154,306.457352396914));
#7052=CARTESIAN_POINT('Ctrl Pts',(-3.08973632633246,2.43351976234868,306.463222086922));
#7053=CARTESIAN_POINT('Ctrl Pts',(-3.16141746537064,2.34250927514171,306.46908590278));
#7054=CARTESIAN_POINT('Ctrl Pts',(-3.22914806794749,2.24823496718569,306.474949718639));
#7055=CARTESIAN_POINT('Ctrl Pts',(-3.29262193170535,2.15107643166227,306.480813534498));
#7056=CARTESIAN_POINT('Ctrl Pts',(-3.35738247842609,2.05194838892828,306.486796216163));
#7057=CARTESIAN_POINT('Ctrl Pts',(-3.41771153372696,1.94981823222956,306.492778897828));
#7058=CARTESIAN_POINT('Ctrl Pts',(-3.47332827271481,1.8451232235165,306.498761579492));
#7059=CARTESIAN_POINT('Ctrl Pts',(-3.52778009104181,1.74262110458731,306.504618950871));
#7060=CARTESIAN_POINT('Ctrl Pts',(-3.5777148678531,1.63766091082651,306.510476322249));
#7061=CARTESIAN_POINT('Ctrl Pts',(-3.6229143175292,1.53067986458368,306.516333693628));
#7062=CARTESIAN_POINT('Ctrl Pts',(-3.66810760446552,1.42371340472087,306.52219026638));
#7063=CARTESIAN_POINT('Ctrl Pts',(-3.70856668768278,1.31472702018849,306.528046839133));
#7064=CARTESIAN_POINT('Ctrl Pts',(-3.74412103833895,1.20417882819275,306.533903411886));
#7065=CARTESIAN_POINT('Ctrl Pts',(-3.77967910680249,1.09361907651796,306.539760597042));
#7066=CARTESIAN_POINT('Ctrl Pts',(-3.81033129686339,0.981497585426619,306.545617782198));
#7067=CARTESIAN_POINT('Ctrl Pts',(-3.83595687098442,0.868287903835731,306.551474967354));
#7068=CARTESIAN_POINT('Ctrl Pts',(-3.86254375848059,0.750831293743016,306.557551877945));
#7069=CARTESIAN_POINT('Ctrl Pts',(-3.88371939351089,0.632203717114054,306.563628788537));
#7070=CARTESIAN_POINT('Ctrl Pts',(-3.89940725364546,0.512944509881105,306.569705699128));
#7071=CARTESIAN_POINT('Ctrl Pts',(-3.91455039755654,0.397826238659985,306.575571606322));
#7072=CARTESIAN_POINT('Ctrl Pts',(-3.92458054935207,0.282119893340267,306.581437513516));
#7073=CARTESIAN_POINT('Ctrl Pts',(-3.92948199990403,0.166313596648635,306.58730342071));
#7074=CARTESIAN_POINT('Ctrl Pts',(-3.93438684269401,0.0504271517399519,
306.593173387631));
#7075=CARTESIAN_POINT('Ctrl Pts',(-3.93415591723505,-0.0655589709785255,
306.599043354553));
#7076=CARTESIAN_POINT('Ctrl Pts',(-3.9288255811531,-0.181158916084803,306.604913321474));
#7077=CARTESIAN_POINT('Ctrl Pts',(-3.92348777435322,-0.296920879977343,
306.610791515432));
#7078=CARTESIAN_POINT('Ctrl Pts',(-3.91303633391891,-0.412295177475449,
306.616669709389));
#7079=CARTESIAN_POINT('Ctrl Pts',(-3.89755913823653,-0.526803344663774,
306.622547903347));
#7080=CARTESIAN_POINT('Ctrl Pts',(-3.89593547204797,-0.538816053115138,
306.623164567048));
#7081=CARTESIAN_POINT('Ctrl Pts',(-3.89425654079538,-0.550819241196603,
306.62378123075));
#7082=CARTESIAN_POINT('Ctrl Pts',(-3.8925224779634,-0.562812365313372,306.624397894451));
#7083=CARTESIAN_POINT('Ctrl Pts',(-3.87595825681001,-0.677373819793196,
306.630288427217));
#7084=CARTESIAN_POINT('Ctrl Pts',(-3.85430596616859,-0.791385236060905,
306.636178959982));
#7085=CARTESIAN_POINT('Ctrl Pts',(-3.82761282970756,-0.904361114742364,
306.642069492747));
#7086=CARTESIAN_POINT('Ctrl Pts',(-3.80095342830771,-1.01719421334313,306.647952580997));
#7087=CARTESIAN_POINT('Ctrl Pts',(-3.76926594581306,-1.12899398134805,306.653835669246));
#7088=CARTESIAN_POINT('Ctrl Pts',(-3.73264916008286,-1.23928174671165,306.659718757496));
#7089=CARTESIAN_POINT('Ctrl Pts',(-3.69606903310955,-1.34945909789509,306.665595955913));
#7090=CARTESIAN_POINT('Ctrl Pts',(-3.65456954905768,-1.45812707048796,306.671473154331));
#7091=CARTESIAN_POINT('Ctrl Pts',(-3.60830001024323,-1.56481948993444,306.677350352749));
#7092=CARTESIAN_POINT('Ctrl Pts',(-3.56123957033372,-1.67333563949662,306.683328012135));
#7093=CARTESIAN_POINT('Ctrl Pts',(-3.50924459489837,-1.77980765438534,306.689305671521));
#7094=CARTESIAN_POINT('Ctrl Pts',(-3.45252449845199,-1.88376314529955,306.695283330907));
#7095=CARTESIAN_POINT('Ctrl Pts',(-3.39681997791561,-1.98585730841461,306.701153960029));
#7096=CARTESIAN_POINT('Ctrl Pts',(-3.3365583500657,-2.08552394555246,306.707024589151));
#7097=CARTESIAN_POINT('Ctrl Pts',(-3.27198525238109,-2.18233854115274,306.712895218274));
#7098=CARTESIAN_POINT('Ctrl Pts',(-3.20742171169672,-2.27913880792032,306.718764978527));
#7099=CARTESIAN_POINT('Ctrl Pts',(-3.13854819798794,-2.37308753135952,306.724634738779));
#7100=CARTESIAN_POINT('Ctrl Pts',(-3.06565409669719,-2.46378853788301,306.730504499032));
#7101=CARTESIAN_POINT('Ctrl Pts',(-2.99275344601327,-2.55449769371547,306.736374786671));
#7102=CARTESIAN_POINT('Ctrl Pts',(-2.91583174676212,-2.6419582326833,306.742245074311));
#7103=CARTESIAN_POINT('Ctrl Pts',(-2.83521871242445,-2.7258070094411,306.74811536195));
#7104=CARTESIAN_POINT('Ctrl Pts',(-2.75202471757622,-2.81234034439038,306.754173596622));
#7105=CARTESIAN_POINT('Ctrl Pts',(-2.66489936305495,-2.89502641257054,306.760231831293));
#7106=CARTESIAN_POINT('Ctrl Pts',(-2.57424524384319,-2.97350810063647,306.766290065965));
#7107=CARTESIAN_POINT('Ctrl Pts',(-2.48627798136556,-3.04966370518938,306.77216874334));
#7108=CARTESIAN_POINT('Ctrl Pts',(-2.3949885424225,-3.12186042568071,306.778047420714));
#7109=CARTESIAN_POINT('Ctrl Pts',(-2.30077659906905,-3.18981442111861,306.783926098089));
#7110=CARTESIAN_POINT('Ctrl Pts',(-2.20224826594791,-3.26088177904689,306.790074111409));
#7111=CARTESIAN_POINT('Ctrl Pts',(-2.10052370290793,-3.32730812825324,306.79622212473));
#7112=CARTESIAN_POINT('Ctrl Pts',(-1.9960904717941,-3.38882159878811,306.80237013805));
#7113=CARTESIAN_POINT('Ctrl Pts',(-1.89165724068026,-3.45033506932299,306.80851815137));
#7114=CARTESIAN_POINT('Ctrl Pts',(-1.78451582035214,-3.50693548322745,306.814666164691));
#7115=CARTESIAN_POINT('Ctrl Pts',(-1.67517794328877,-3.55840805112607,306.820814178011));
#7116=CARTESIAN_POINT('Ctrl Pts',(-1.57185477980409,-3.60704909566439,306.82662398704));
#7117=CARTESIAN_POINT('Ctrl Pts',(-1.46622651812633,-3.65127302112401,306.832433796069));
#7118=CARTESIAN_POINT('Ctrl Pts',(-1.35871205605211,-3.69085227945236,306.838243605099));
#7119=CARTESIAN_POINT('Ctrl Pts',(-1.25133244258961,-3.73038189601218,306.844046127251));
#7120=CARTESIAN_POINT('Ctrl Pts',(-1.14207172465273,-3.76527828081848,306.849848649403));
#7121=CARTESIAN_POINT('Ctrl Pts',(-1.03137203581375,-3.79536042079555,306.855651171555));
#7122=CARTESIAN_POINT('Ctrl Pts',(-0.916699611110698,-3.82652213378325,
306.861661931762));
#7123=CARTESIAN_POINT('Ctrl Pts',(-0.800483396006691,-3.8525173513266,306.867672691969));
#7124=CARTESIAN_POINT('Ctrl Pts',(-0.683236457770158,-3.87319983253817,
306.873683452175));
#7125=CARTESIAN_POINT('Ctrl Pts',(-0.570238634224967,-3.89313276552194,
306.879476378041));
#7126=CARTESIAN_POINT('Ctrl Pts',(-0.456283954458853,-3.90813126031801,
306.885269303907));
#7127=CARTESIAN_POINT('Ctrl Pts',(-0.341844866762429,-3.91811575723181,
306.891062229773));
#7128=CARTESIAN_POINT('Ctrl Pts',(-0.227442596936768,-3.92809704188724,
306.896853291912));
#7129=CARTESIAN_POINT('Ctrl Pts',(-0.112556649794527,-3.93306749798193,
306.902644354051));
#7130=CARTESIAN_POINT('Ctrl Pts',(0.0023343352513748,-3.93299930725635,
306.908435416191));
#7131=CARTESIAN_POINT('Ctrl Pts',(0.117217598358397,-3.93293112111394,306.914226089107));
#7132=CARTESIAN_POINT('Ctrl Pts',(0.232105475818189,-3.92782496247348,306.920016762023));
#7133=CARTESIAN_POINT('Ctrl Pts',(0.346519097391488,-3.91770513376683,306.925807434939));
#7134=CARTESIAN_POINT('Ctrl Pts',(0.46095415010996,-3.90758340948591,306.931599192522));
#7135=CARTESIAN_POINT('Ctrl Pts',(0.574914349355133,-3.89244618727576,306.937390950106));
#7136=CARTESIAN_POINT('Ctrl Pts',(0.687926557494139,-3.87236956545915,306.94318270769));
#7137=CARTESIAN_POINT('Ctrl Pts',(0.801046495301565,-3.85227380546404,306.948979986306));
#7138=CARTESIAN_POINT('Ctrl Pts',(0.913216221904416,-3.82722932348057,306.954777264923));
#7139=CARTESIAN_POINT('Ctrl Pts',(1.02397351037318,-3.79736319701632,306.96057454354));
#7140=CARTESIAN_POINT('Ctrl Pts',(1.13479391769831,-3.76748005031103,306.966375125935));
#7141=CARTESIAN_POINT('Ctrl Pts',(1.24419988250263,-3.73276991765602,306.972175708331));
#7142=CARTESIAN_POINT('Ctrl Pts',(1.35174671657435,-3.69340896926274,306.977976290726));
#7143=CARTESIAN_POINT('Ctrl Pts',(1.45943800980113,-3.65399515042101,306.983784664585));
#7144=CARTESIAN_POINT('Ctrl Pts',(1.56526480094117,-3.60991821374187,306.989593038445));
#7145=CARTESIAN_POINT('Ctrl Pts',(1.66880475645938,-3.56140136530812,306.995401412304));
#7146=CARTESIAN_POINT('Ctrl Pts',(1.69559128725737,-3.54884970785098,306.996904080375));
#7147=CARTESIAN_POINT('Ctrl Pts',(1.72222490323772,-3.53600112129244,306.998406748446));
#7148=CARTESIAN_POINT('Ctrl Pts',(1.74869860048799,-3.52285994678348,306.999909416517));
#7149=CARTESIAN_POINT('',(-1.74869447533106,-3.52286199445091,307.));
#7150=CARTESIAN_POINT('Origin',(0.,0.,307.));
#7151=CARTESIAN_POINT('',(3.93127820247977,0.00326437435658078,306.154164236595));
#7152=CARTESIAN_POINT('Ctrl Pts',(-1.74869447533129,-3.5228619944508,307.));
#7153=CARTESIAN_POINT('Ctrl Pts',(-2.90806357314774,-2.94736901759987,306.93452790548));
#7154=CARTESIAN_POINT('Ctrl Pts',(-4.59459704467384,-0.57010578582661,306.80358371644));
#7155=CARTESIAN_POINT('Ctrl Pts',(-3.00810365225817,3.52651283114026,306.60716743288));
#7156=CARTESIAN_POINT('Ctrl Pts',(1.28568539453312,4.45038130233524,306.410751149319));
#7157=CARTESIAN_POINT('Ctrl Pts',(3.69704862595707,2.09019977571459,306.259750186429));
#7158=CARTESIAN_POINT('Ctrl Pts',(3.93358950080438,0.400386139161716,306.174221318059));
#7159=CARTESIAN_POINT('Ctrl Pts',(3.93053755798013,0.00326985260832528,
306.154164544208));
#7160=CARTESIAN_POINT('',(3.932998918852,-0.0029162148394918,304.904163521999));
#7161=CARTESIAN_POINT('Ctrl Pts',(3.93299865583244,0.00325164884982929,
306.154163522035));
#7162=CARTESIAN_POINT('Ctrl Pts',(3.93309417218823,-0.11227918374711,306.148332127252));
#7163=CARTESIAN_POINT('Ctrl Pts',(3.9280948765027,-0.227892259450327,306.142500732469));
#7164=CARTESIAN_POINT('Ctrl Pts',(3.91800580906771,-0.34310272530493,306.136669337686));
#7165=CARTESIAN_POINT('Ctrl Pts',(3.9079197792971,-0.458278503044824,306.130839698647));
#7166=CARTESIAN_POINT('Ctrl Pts',(3.89274706022665,-0.573051497308586,306.125010059608));
#7167=CARTESIAN_POINT('Ctrl Pts',(3.87254472272492,-0.686939859445751,306.119180420569));
#7168=CARTESIAN_POINT('Ctrl Pts',(3.85234348722245,-0.800822009188452,306.113351099526));
#7169=CARTESIAN_POINT('Ctrl Pts',(3.82711325170791,-0.913819212630393,306.107521778483));
#7170=CARTESIAN_POINT('Ctrl Pts',(3.79696245960987,-1.02545847322716,306.101692457439));
#7171=CARTESIAN_POINT('Ctrl Pts',(3.76680587879097,-1.13711916770582,306.095862017211));
#7172=CARTESIAN_POINT('Ctrl Pts',(3.73172697215613,-1.24742099899279,306.090031576983));
#7173=CARTESIAN_POINT('Ctrl Pts',(3.69188422433854,-1.35590555500013,306.084201136755));
#7174=CARTESIAN_POINT('Ctrl Pts',(3.65199908332218,-1.46450553997756,306.078364492863));
#7175=CARTESIAN_POINT('Ctrl Pts',(3.6073401226729,-1.57128399664453,306.072527848971));
#7176=CARTESIAN_POINT('Ctrl Pts',(3.55811428393509,-1.67580182075837,306.06669120508));
#7177=CARTESIAN_POINT('Ctrl Pts',(3.50886108750736,-1.78037773156605,306.060851317422));
#7178=CARTESIAN_POINT('Ctrl Pts',(3.45503615222371,-1.88269013933472,306.055011429764));
#7179=CARTESIAN_POINT('Ctrl Pts',(3.39689187124467,-1.98232555728666,306.049171542107));
#7180=CARTESIAN_POINT('Ctrl Pts',(3.3386534669034,-2.08212226402534,306.043322200899));
#7181=CARTESIAN_POINT('Ctrl Pts',(3.27608197580863,-2.17923297481225,306.037472859691));
#7182=CARTESIAN_POINT('Ctrl Pts',(3.20947272689476,-2.27327381001909,306.031623518484));
#7183=CARTESIAN_POINT('Ctrl Pts',(3.15745116982446,-2.34671932630132,306.027055206389));
#7184=CARTESIAN_POINT('Ctrl Pts',(3.10296764191761,-2.4182929457685,306.022486894294));
#7185=CARTESIAN_POINT('Ctrl Pts',(3.04617884903102,-2.48782704779011,306.017918582199));
#7186=CARTESIAN_POINT('Ctrl Pts',(2.97306129458837,-2.57735463293069,306.012036720808));
#7187=CARTESIAN_POINT('Ctrl Pts',(2.89587579309586,-2.66380029440954,306.006154859417));
#7188=CARTESIAN_POINT('Ctrl Pts',(2.81491173847977,-2.74677281633717,306.000272998026));
#7189=CARTESIAN_POINT('Ctrl Pts',(2.73405006001075,-2.82964042248275,305.994398574038));
#7190=CARTESIAN_POINT('Ctrl Pts',(2.64941961592671,-2.90904333128066,305.98852415005));
#7191=CARTESIAN_POINT('Ctrl Pts',(2.56135051466587,-2.98462267984093,305.982649726062));
#7192=CARTESIAN_POINT('Ctrl Pts',(2.47336944781431,-3.0601264788247,305.976781174184));
#7193=CARTESIAN_POINT('Ctrl Pts',(2.38195687220633,-3.13181405399361,305.970912622306));
#7194=CARTESIAN_POINT('Ctrl Pts',(2.28747980121963,-3.19936324274256,305.965044070428));
#7195=CARTESIAN_POINT('Ctrl Pts',(2.19119393685813,-3.2682056820528,305.95906316327));
#7196=CARTESIAN_POINT('Ctrl Pts',(2.09172533096063,-3.33274933108614,305.953082256113));
#7197=CARTESIAN_POINT('Ctrl Pts',(1.98949827718364,-3.39269591992612,305.947101348955));
#7198=CARTESIAN_POINT('Ctrl Pts',(1.88930221312591,-3.45145152359006,305.941239267103));
#7199=CARTESIAN_POINT('Ctrl Pts',(1.78645666748683,-3.50579082792641,305.935377185251));
#7200=CARTESIAN_POINT('Ctrl Pts',(1.68138986744675,-3.55547705851794,305.929515103399));
#7201=CARTESIAN_POINT('Ctrl Pts',(1.57633770137118,-3.60515636868805,305.923653838033));
#7202=CARTESIAN_POINT('Ctrl Pts',(1.46906526829634,-3.65018371799922,305.917792572666));
#7203=CARTESIAN_POINT('Ctrl Pts',(1.36002368258499,-3.6903691661957,305.911931307299));
#7204=CARTESIAN_POINT('Ctrl Pts',(1.25097113359423,-3.730558654725,305.906069452629));
#7205=CARTESIAN_POINT('Ctrl Pts',(1.14014946472176,-3.76590513201227,305.900207597958));
#7206=CARTESIAN_POINT('Ctrl Pts',(1.02802731453032,-3.79626775143424,305.894345743287));
#7207=CARTESIAN_POINT('Ctrl Pts',(0.911918390824577,-3.82770998703133,305.888275456233));
#7208=CARTESIAN_POINT('Ctrl Pts',(0.794415239715369,-3.8538072136957,305.882205169179));
#7209=CARTESIAN_POINT('Ctrl Pts',(0.676051153361322,-3.87446045766876,305.876134882125));
#7210=CARTESIAN_POINT('Ctrl Pts',(0.561583168810041,-3.89443387430944,305.870264406154));
#7211=CARTESIAN_POINT('Ctrl Pts',(0.446310457463014,-3.90931606797126,305.864393930184));
#7212=CARTESIAN_POINT('Ctrl Pts',(0.330720679943943,-3.91907040404449,305.858523454213));
#7213=CARTESIAN_POINT('Ctrl Pts',(0.209229476681172,-3.92932274687273,305.852353261617));
#7214=CARTESIAN_POINT('Ctrl Pts',(0.0873885057713353,-3.93390978712592,
305.846183069022));
#7215=CARTESIAN_POINT('Ctrl Pts',(-0.0342373266273185,-3.93285097676805,
305.840012876426));
#7216=CARTESIAN_POINT('Ctrl Pts',(-0.155863159025963,-3.93179216641018,
305.83384268383));
#7217=CARTESIAN_POINT('Ctrl Pts',(-0.277273336903729,-3.92508760441031,
305.827672491235));
#7218=CARTESIAN_POINT('Ctrl Pts',(-0.397912032186795,-3.912819317914,305.821502298639));
#7219=CARTESIAN_POINT('Ctrl Pts',(-0.512921609468159,-3.90112348151096,
305.815620013187));
#7220=CARTESIAN_POINT('Ctrl Pts',(-0.627599793355764,-3.88433385812013,
305.809737727736));
#7221=CARTESIAN_POINT('Ctrl Pts',(-0.741460588139995,-3.86247656254832,
305.803855442284));
#7222=CARTESIAN_POINT('Ctrl Pts',(-0.855177774889915,-3.84064683470304,
305.797980575922));
#7223=CARTESIAN_POINT('Ctrl Pts',(-0.968079222106158,-3.81376222373203,
305.79210570956));
#7224=CARTESIAN_POINT('Ctrl Pts',(-1.07968351999496,-3.78190064605765,305.786230843198));
#7225=CARTESIAN_POINT('Ctrl Pts',(-1.19117660146453,-3.75007081922663,305.780361831284));
#7226=CARTESIAN_POINT('Ctrl Pts',(-1.30137471136452,-3.71327400422141,305.774492819371));
#7227=CARTESIAN_POINT('Ctrl Pts',(-1.40980675142425,-3.6716391330901,305.768623807457));
#7228=CARTESIAN_POINT('Ctrl Pts',(-1.52030303173504,-3.62921165142789,305.762643066108));
#7229=CARTESIAN_POINT('Ctrl Pts',(-1.62896488516239,-3.58176010348318,305.756662324759));
#7230=CARTESIAN_POINT('Ctrl Pts',(-1.73530976509467,-3.52947432618047,305.75068158341));
#7231=CARTESIAN_POINT('Ctrl Pts',(-1.83955364071031,-3.47822153367103,305.744819000673));
#7232=CARTESIAN_POINT('Ctrl Pts',(-1.9415708682392,-3.42232396481679,305.738956417935));
#7233=CARTESIAN_POINT('Ctrl Pts',(-2.04092790802344,-3.36200866659369,305.733093835198));
#7234=CARTESIAN_POINT('Ctrl Pts',(-2.14027135466279,-3.30170162017227,305.727232054527));
#7235=CARTESIAN_POINT('Ctrl Pts',(-2.23695498551482,-3.23697825992387,305.721370273856));
#7236=CARTESIAN_POINT('Ctrl Pts',(-2.33057174777083,-3.16811052971521,305.715508493186));
#7237=CARTESIAN_POINT('Ctrl Pts',(-2.42419814361127,-3.09923571270845,305.709646109311));
#7238=CARTESIAN_POINT('Ctrl Pts',(-2.51475671185153,-3.02621592187917,305.703783725437));
#7239=CARTESIAN_POINT('Ctrl Pts',(-2.60187172518877,-2.94936476646468,305.697921341562));
#7240=CARTESIAN_POINT('Ctrl Pts',(-2.69206612639077,-2.86979703549896,305.691851731022));
#7241=CARTESIAN_POINT('Ctrl Pts',(-2.7785686586941,-2.78612237288855,305.685782120482));
#7242=CARTESIAN_POINT('Ctrl Pts',(-2.86100315466831,-2.69873117389969,305.679712509941));
#7243=CARTESIAN_POINT('Ctrl Pts',(-2.94074069765388,-2.61419909295975,305.673841474695));
#7244=CARTESIAN_POINT('Ctrl Pts',(-3.01667199864521,-2.52619021322746,305.667970439449));
#7245=CARTESIAN_POINT('Ctrl Pts',(-3.08849782474958,-2.43509141235337,305.662099404203));
#7246=CARTESIAN_POINT('Ctrl Pts',(-3.16396768481436,-2.3393707763798,305.655930506016));
#7247=CARTESIAN_POINT('Ctrl Pts',(-3.23490425767385,-2.24023889389887,305.649761607828));
#7248=CARTESIAN_POINT('Ctrl Pts',(-3.30101282934007,-2.13817756524857,305.643592709641));
#7249=CARTESIAN_POINT('Ctrl Pts',(-3.36712140100628,-2.03611623659827,305.637423811454));
#7250=CARTESIAN_POINT('Ctrl Pts',(-3.42840177023318,-1.93112594615363,305.631254913266));
#7251=CARTESIAN_POINT('Ctrl Pts',(-3.48461637982025,-1.82371535210087,305.625086015079));
#7252=CARTESIAN_POINT('Ctrl Pts',(-3.53820812030988,-1.72131633653185,305.619204946204));
#7253=CARTESIAN_POINT('Ctrl Pts',(-3.58736886382915,-1.61638783416557,305.613323877329));
#7254=CARTESIAN_POINT('Ctrl Pts',(-3.63185255390124,-1.50934953762243,305.607442808454));
#7255=CARTESIAN_POINT('Ctrl Pts',(-3.67627997401797,-1.4024466399223,305.601569178878));
#7256=CARTESIAN_POINT('Ctrl Pts',(-3.71604195049381,-1.29343963291238,305.595695549302));
#7257=CARTESIAN_POINT('Ctrl Pts',(-3.75093817048656,-1.18277294574526,305.589821919726));
#7258=CARTESIAN_POINT('Ctrl Pts',(-3.78579949819037,-1.07221691279875,305.583954163119));
#7259=CARTESIAN_POINT('Ctrl Pts',(-3.81580462436139,-0.960004891458814,
305.578086406511));
#7260=CARTESIAN_POINT('Ctrl Pts',(-3.84080148226255,-0.846600835016009,
305.572218649903));
#7261=CARTESIAN_POINT('Ctrl Pts',(-3.86628163417958,-0.731004202927437,
305.56623744497));
#7262=CARTESIAN_POINT('Ctrl Pts',(-3.88655767673246,-0.614169364116873,
305.560256240037));
#7263=CARTESIAN_POINT('Ctrl Pts',(-3.90152196282265,-0.496603839707777,
305.554275035105));
#7264=CARTESIAN_POINT('Ctrl Pts',(-3.91618623511738,-0.381395345829929,
305.548413745281));
#7265=CARTESIAN_POINT('Ctrl Pts',(-3.92574969970113,-0.265485618831752,
305.542552455457));
#7266=CARTESIAN_POINT('Ctrl Pts',(-3.93016286975356,-0.149361364517402,
305.536691165633));
#7267=CARTESIAN_POINT('Ctrl Pts',(-3.93457542705394,-0.0332532336183861,
305.530830689627));
#7268=CARTESIAN_POINT('Ctrl Pts',(-3.93383909629661,0.0830689538829383,
305.524970213621));
#7269=CARTESIAN_POINT('Ctrl Pts',(-3.92795645087036,0.199115845843437,305.519109737615));
#7270=CARTESIAN_POINT('Ctrl Pts',(-3.92207321030637,0.315174478080568,305.513248668714));
#7271=CARTESIAN_POINT('Ctrl Pts',(-3.91104264093404,0.430957348054308,305.507387599813));
#7272=CARTESIAN_POINT('Ctrl Pts',(-3.89491934697215,0.545978278489179,305.501526530912));
#7273=CARTESIAN_POINT('Ctrl Pts',(-3.87821745047479,0.665126864361013,305.495455130963));
#7274=CARTESIAN_POINT('Ctrl Pts',(-3.8560505118387,0.783457324639823,305.489383731013));
#7275=CARTESIAN_POINT('Ctrl Pts',(-3.82853716399658,0.900439994612101,305.483312331064));
#7276=CARTESIAN_POINT('Ctrl Pts',(-3.80193781613805,1.01353647236053,305.47744262447));
#7277=CARTESIAN_POINT('Ctrl Pts',(-3.77034180769444,1.12537289937087,305.471572917876));
#7278=CARTESIAN_POINT('Ctrl Pts',(-3.73390706277148,1.23548656268909,305.465703211282));
#7279=CARTESIAN_POINT('Ctrl Pts',(-3.69559437577795,1.35127577228398,305.459530964655));
#7280=CARTESIAN_POINT('Ctrl Pts',(-3.65193105163972,1.46515940023407,305.453358718027));
#7281=CARTESIAN_POINT('Ctrl Pts',(-3.60315728430097,1.57662506151235,305.4471864714));
#7282=CARTESIAN_POINT('Ctrl Pts',(-3.55438351696223,1.68809072279065,305.441014224773));
#7283=CARTESIAN_POINT('Ctrl Pts',(-3.50049960109066,1.79713798072305,305.434841978145));
#7284=CARTESIAN_POINT('Ctrl Pts',(-3.44179979713586,1.90328746027381,305.428669731518));
#7285=CARTESIAN_POINT('Ctrl Pts',(-3.38586408005447,2.00443851796832,305.422788126847));
#7286=CARTESIAN_POINT('Ctrl Pts',(-3.32537540815491,2.10328456815501,305.416906522177));
#7287=CARTESIAN_POINT('Ctrl Pts',(-3.26054857752851,2.19938900005815,305.411024917506));
#7288=CARTESIAN_POINT('Ctrl Pts',(-3.19580367231638,2.29537197923376,305.405150745759));
#7289=CARTESIAN_POINT('Ctrl Pts',(-3.12673174029815,2.38861989252677,305.399276574013));
#7290=CARTESIAN_POINT('Ctrl Pts',(-3.05359341895139,2.47872068449367,305.393402402266));
#7291=CARTESIAN_POINT('Ctrl Pts',(-2.98052815062925,2.56873148074762,305.38753409784));
#7292=CARTESIAN_POINT('Ctrl Pts',(-2.90340483073116,2.6556010908894,305.381665793415));
#7293=CARTESIAN_POINT('Ctrl Pts',(-2.82252696655011,2.73894697340008,305.375797488989));
#7294=CARTESIAN_POINT('Ctrl Pts',(-2.74009589125975,2.82389346383904,305.369816487279));
#7295=CARTESIAN_POINT('Ctrl Pts',(-2.6537648180976,2.90517912670088,305.36383548557));
#7296=CARTESIAN_POINT('Ctrl Pts',(-2.56389794442153,2.98243463140285,305.35785448386));
#7297=CARTESIAN_POINT('Ctrl Pts',(-2.47582140148219,3.05815104946487,305.351992635858));
#7298=CARTESIAN_POINT('Ctrl Pts',(-2.38434896132091,3.12999612110749,305.346130787856));
#7299=CARTESIAN_POINT('Ctrl Pts',(-2.28985962129222,3.19766038140004,305.340268939854));
#7300=CARTESIAN_POINT('Ctrl Pts',(-2.19538335324821,3.26531528078296,305.334407902801));
#7301=CARTESIAN_POINT('Ctrl Pts',(-2.09789135007304,3.32879027936651,305.328546865747));
#7302=CARTESIAN_POINT('Ctrl Pts',(-1.99779349631778,3.38781790332219,305.322685828694));
#7303=CARTESIAN_POINT('Ctrl Pts',(-1.89768547854856,3.44685152098875,305.316824196506));
#7304=CARTESIAN_POINT('Ctrl Pts',(-1.79497143890895,3.50143665712838,305.310962564319));
#7305=CARTESIAN_POINT('Ctrl Pts',(-1.6900872756754,3.55135101061555,305.305100932131));
#7306=CARTESIAN_POINT('Ctrl Pts',(-1.58146355710944,3.60304501777962,305.29903030845));
#7307=CARTESIAN_POINT('Ctrl Pts',(-1.47051250808343,3.64972875318375,305.292959684769));
#7308=CARTESIAN_POINT('Ctrl Pts',(-1.35774125846145,3.69120951384116,305.286889061088));
#7309=CARTESIAN_POINT('Ctrl Pts',(-1.24869188428673,3.7313212533594,305.281018790824));
#7310=CARTESIAN_POINT('Ctrl Pts',(-1.13794097813819,3.76656796712536,305.27514852056));
#7311=CARTESIAN_POINT('Ctrl Pts',(-1.02596177403602,3.79682649566936,305.269278250296));
#7312=CARTESIAN_POINT('Ctrl Pts',(-0.908249763301447,3.82863411803407,305.263107449907));
#7313=CARTESIAN_POINT('Ctrl Pts',(-0.789180877071169,3.85492918090016,305.256936649517));
#7314=CARTESIAN_POINT('Ctrl Pts',(-0.669314587155635,3.87562988215086,305.250765849127));
#7315=CARTESIAN_POINT('Ctrl Pts',(-0.54944829724011,3.89633058340156,305.244595048737));
#7316=CARTESIAN_POINT('Ctrl Pts',(-0.428785129427652,3.91143692830187,305.238424248348));
#7317=CARTESIAN_POINT('Ctrl Pts',(-0.307886798320349,3.92093033850642,305.232253447958));
#7318=CARTESIAN_POINT('Ctrl Pts',(-0.192654566553249,3.92997882441132,305.226371852289));
#7319=CARTESIAN_POINT('Ctrl Pts',(-0.0768375312944448,3.9339577482393,305.220490256619));
#7320=CARTESIAN_POINT('Ctrl Pts',(0.0390815966009194,3.93280582139611,305.21460866095));
#7321=CARTESIAN_POINT('Ctrl Pts',(0.154854253226902,3.93165535008653,305.208734497054));
#7322=CARTESIAN_POINT('Ctrl Pts',(0.270728337701162,3.92538692618264,305.202860333159));
#7323=CARTESIAN_POINT('Ctrl Pts',(0.386216376054573,3.9139910463448,305.196986169264));
#7324=CARTESIAN_POINT('Ctrl Pts',(0.501589083605886,3.90260654687138,305.191117871535));
#7325=CARTESIAN_POINT('Ctrl Pts',(0.616576104422988,3.88610481763749,305.185249573805));
#7326=CARTESIAN_POINT('Ctrl Pts',(0.730690976763123,3.86452839250496,305.179381276076));
#7327=CARTESIAN_POINT('Ctrl Pts',(0.846997547081014,3.84253756908796,305.173400271423));
#7328=CARTESIAN_POINT('Ctrl Pts',(0.962397687329678,3.81527511124227,305.16741926677));
#7329=CARTESIAN_POINT('Ctrl Pts',(1.07638252241415,3.78284148034799,305.161438262117));
#7330=CARTESIAN_POINT('Ctrl Pts',(1.1880964209889,3.75105402941691,305.155576417892));
#7331=CARTESIAN_POINT('Ctrl Pts',(1.29845047356426,3.71429966859478,305.149714573668));
#7332=CARTESIAN_POINT('Ctrl Pts',(1.40697761397419,3.67272419244564,305.143852729443));
#7333=CARTESIAN_POINT('Ctrl Pts',(1.51548976076468,3.63115446017646,305.137991695065));
#7334=CARTESIAN_POINT('Ctrl Pts',(1.62217511289051,3.5847650844574,305.132130660686));
#7335=CARTESIAN_POINT('Ctrl Pts',(1.72658463093574,3.53375077109528,305.126269626308));
#7336=CARTESIAN_POINT('Ctrl Pts',(1.8310047706039,3.48273126802622,305.120407995684));
#7337=CARTESIAN_POINT('Ctrl Pts',(1.9331482459501,3.42708607278105,305.11454636506));
#7338=CARTESIAN_POINT('Ctrl Pts',(2.03258938448524,3.36705648810321,305.108684734436));
#7339=CARTESIAN_POINT('Ctrl Pts',(2.13557616081782,3.30488650994704,305.1026141036));
#7340=CARTESIAN_POINT('Ctrl Pts',(2.23566388700295,3.23801389423704,305.096543472763));
#7341=CARTESIAN_POINT('Ctrl Pts',(2.33241234604614,3.16675569755728,305.090472841926));
#7342=CARTESIAN_POINT('Ctrl Pts',(2.4259676516519,3.0978493559657,305.084602570413));
#7343=CARTESIAN_POINT('Ctrl Pts',(2.51640034868806,3.02484266621994,305.078732298899));
#7344=CARTESIAN_POINT('Ctrl Pts',(2.60334693356386,2.94806271023933,305.072862027385));
#7345=CARTESIAN_POINT('Ctrl Pts',(2.69474490339167,2.86735186794321,305.066691216887));
#7346=CARTESIAN_POINT('Ctrl Pts',(2.78228997826085,2.78247154443906,305.060520406389));
#7347=CARTESIAN_POINT('Ctrl Pts',(2.86560565657207,2.69384357768267,305.054349595891));
#7348=CARTESIAN_POINT('Ctrl Pts',(2.94892133488328,2.60521561092629,305.048178785394));
#7349=CARTESIAN_POINT('Ctrl Pts',(3.02800733135905,2.51284044262219,305.042007974896));
#7350=CARTESIAN_POINT('Ctrl Pts',(3.10253867254258,2.4171766144363,305.035837164398));
#7351=CARTESIAN_POINT('Ctrl Pts',(3.17348408456588,2.32611546353521,305.029963250333));
#7352=CARTESIAN_POINT('Ctrl Pts',(3.24053631565406,2.23177517989596,305.024089336267));
#7353=CARTESIAN_POINT('Ctrl Pts',(3.30337740364183,2.13452259981209,305.018215422202));
#7354=CARTESIAN_POINT('Ctrl Pts',(3.36614122950051,2.03738959024549,305.012348730021));
#7355=CARTESIAN_POINT('Ctrl Pts',(3.42470398349916,1.93735174536747,305.006482037841));
#7356=CARTESIAN_POINT('Ctrl Pts',(3.47878801540304,1.83480869408452,305.000615345661));
#7357=CARTESIAN_POINT('Ctrl Pts',(3.53281858841152,1.73236700059722,304.994754452361));
#7358=CARTESIAN_POINT('Ctrl Pts',(3.58237905098065,1.62742538710442,304.988893559062));
#7359=CARTESIAN_POINT('Ctrl Pts',(3.62723552917024,1.52041159424843,304.983032665763));
#7360=CARTESIAN_POINT('Ctrl Pts',(3.67205847953301,1.41347778849932,304.97717615317));
#7361=CARTESIAN_POINT('Ctrl Pts',(3.71218428023923,1.3044752631427,304.971319640576));
#7362=CARTESIAN_POINT('Ctrl Pts',(3.74742573860542,1.19385482100531,304.965463127982));
#7363=CARTESIAN_POINT('Ctrl Pts',(3.78265198772662,1.08328211961088,304.959609142899));
#7364=CARTESIAN_POINT('Ctrl Pts',(3.81299796052456,0.971093282010455,304.953755157815));
#7365=CARTESIAN_POINT('Ctrl Pts',(3.83832542279738,0.857756928685132,304.947901172731));
#7366=CARTESIAN_POINT('Ctrl Pts',(3.86364640261167,0.744449583327597,304.94204868595));
#7367=CARTESIAN_POINT('Ctrl Pts',(3.88395134062945,0.629995709581894,304.93619619917));
#7368=CARTESIAN_POINT('Ctrl Pts',(3.89915268039494,0.514876077293334,304.930343712389));
#7369=CARTESIAN_POINT('Ctrl Pts',(3.91435720086164,0.399732357578294,304.924490001044));
#7370=CARTESIAN_POINT('Ctrl Pts',(3.92445593538042,0.283923010003483,304.9186362897));
#7371=CARTESIAN_POINT('Ctrl Pts',(3.92941301624533,0.167935546450875,304.912782578355));
#7372=CARTESIAN_POINT('Ctrl Pts',(3.93184596613777,0.111008557631404,304.909909559582));
#7373=CARTESIAN_POINT('Ctrl Pts',(3.93304114942374,0.054038722546335,304.907036540808));
#7374=CARTESIAN_POINT('Ctrl Pts',(3.93299891885253,-0.00291621412706657,
304.904163522035));
#7375=CARTESIAN_POINT('',(3.93299992201116,0.000783236989828259,303.654163521989));
#7376=CARTESIAN_POINT('Ctrl Pts',(3.932998918852,-0.00291621483949189,304.904163521999));
#7377=CARTESIAN_POINT('Ctrl Pts',(3.93289858185281,-0.138237283777497,304.897337424136));
#7378=CARTESIAN_POINT('Ctrl Pts',(3.92581040854498,-0.273276789480336,304.890511326274));
#7379=CARTESIAN_POINT('Ctrl Pts',(3.91184495515244,-0.40737948751549,304.883685228411));
#7380=CARTESIAN_POINT('Ctrl Pts',(3.8977947592586,-0.542295921971808,304.876817709723));
#7381=CARTESIAN_POINT('Ctrl Pts',(3.87678367602707,-0.676264042733198,304.869950191035));
#7382=CARTESIAN_POINT('Ctrl Pts',(3.84897348829923,-0.80863594179929,304.863082672347));
#7383=CARTESIAN_POINT('Ctrl Pts',(3.82098188003345,-0.941871372653556,304.856170353208));
#7384=CARTESIAN_POINT('Ctrl Pts',(3.78610224826225,-1.07348958982204,304.84925803407));
#7385=CARTESIAN_POINT('Ctrl Pts',(3.74454784416664,-1.20285096447855,304.842345714931));
#7386=CARTESIAN_POINT('Ctrl Pts',(3.73868682341047,-1.22109667677811,304.841370770234));
#7387=CARTESIAN_POINT('Ctrl Pts',(3.73269309461101,-1.2392975278324,304.840395825536));
#7388=CARTESIAN_POINT('Ctrl Pts',(3.72656733149945,-1.25745175804126,304.839420880838));
#7389=CARTESIAN_POINT('Ctrl Pts',(3.68961247830752,-1.36697067021004,304.833539337996));
#7390=CARTESIAN_POINT('Ctrl Pts',(3.64776609021771,-1.47503554230942,304.827657795155));
#7391=CARTESIAN_POINT('Ctrl Pts',(3.60116145689045,-1.58117840910084,304.821776252313));
#7392=CARTESIAN_POINT('Ctrl Pts',(3.55461572171183,-1.68718713432952,304.815902142466));
#7393=CARTESIAN_POINT('Ctrl Pts',(3.50332386513835,-1.79127831134769,304.810028032619));
#7394=CARTESIAN_POINT('Ctrl Pts',(3.44746866921305,-1.89299994051621,304.804153922772));
#7395=CARTESIAN_POINT('Ctrl Pts',(3.39166926383829,-1.99461996578561,304.798285680236));
#7396=CARTESIAN_POINT('Ctrl Pts',(3.33131578337192,-2.09387479244845,304.7924174377));
#7397=CARTESIAN_POINT('Ctrl Pts',(3.26663846483617,-2.19033379649149,304.786549195164));
#7398=CARTESIAN_POINT('Ctrl Pts',(3.20071810605026,-2.28864665637192,304.780568170252));
#7399=CARTESIAN_POINT('Ctrl Pts',(3.13030616592147,-2.38405471880515,304.77458714534));
#7400=CARTESIAN_POINT('Ctrl Pts',(3.05569496827276,-2.47612949194353,304.768606120428));
#7401=CARTESIAN_POINT('Ctrl Pts',(2.98257122751017,-2.5663686524707,304.762744333874));
#7402=CARTESIAN_POINT('Ctrl Pts',(2.90541438336051,-2.65340586451198,304.75688254732));
#7403=CARTESIAN_POINT('Ctrl Pts',(2.82454200990618,-2.7368689106852,304.751020760766));
#7404=CARTESIAN_POINT('Ctrl Pts',(2.74368082089702,-2.82032041412975,304.745159784883));
#7405=CARTESIAN_POINT('Ctrl Pts',(2.65910541096222,-2.90019843905125,304.739298808999));
#7406=CARTESIAN_POINT('Ctrl Pts',(2.57117124949181,-2.97616656217133,304.733437833115));
#7407=CARTESIAN_POINT('Ctrl Pts',(2.48322815377449,-3.0521424037703,304.727576261747));
#7408=CARTESIAN_POINT('Ctrl Pts',(2.39192593975536,-3.12420728464715,304.721714690379));
#7409=CARTESIAN_POINT('Ctrl Pts',(2.29765374571631,-3.19206457716567,304.715853119011));
#7410=CARTESIAN_POINT('Ctrl Pts',(2.20001795340542,-3.26234299368764,304.709782408867));
#7411=CARTESIAN_POINT('Ctrl Pts',(2.09919667238236,-3.32810768296923,304.703711698722));
#7412=CARTESIAN_POINT('Ctrl Pts',(1.99565444942337,-3.38907838777694,304.697640988578));
#7413=CARTESIAN_POINT('Ctrl Pts',(1.89553194798443,-3.44803539396618,304.691770777684));
#7414=CARTESIAN_POINT('Ctrl Pts',(1.7928657960717,-3.50250993923882,304.68590056679));
#7415=CARTESIAN_POINT('Ctrl Pts',(1.68809958710319,-3.55229626917886,304.680030355896));
#7416=CARTESIAN_POINT('Ctrl Pts',(1.57796588450083,-3.60463330522573,304.673859396126));
#7417=CARTESIAN_POINT('Ctrl Pts',(1.46551172948751,-3.65178881521169,304.667688436356));
#7418=CARTESIAN_POINT('Ctrl Pts',(1.35127301287926,-3.69358230511575,304.661517476586));
#7419=CARTESIAN_POINT('Ctrl Pts',(1.23703429627102,-3.73537579501982,304.655346516817));
#7420=CARTESIAN_POINT('Ctrl Pts',(1.12101153643795,-3.77180717603904,304.649175557047));
#7421=CARTESIAN_POINT('Ctrl Pts',(1.0037541319802,-3.80275776805895,304.643004597277));
#7422=CARTESIAN_POINT('Ctrl Pts',(0.891996200861796,-3.83225675063519,304.637123060839));
#7423=CARTESIAN_POINT('Ctrl Pts',(0.778756740574146,-3.85687246499804,304.631241524402));
#7424=CARTESIAN_POINT('Ctrl Pts',(0.664499721253345,-3.87645832177443,304.625359987964));
#7425=CARTESIAN_POINT('Ctrl Pts',(0.550387097470445,-3.89601942637068,304.619485884484));
#7426=CARTESIAN_POINT('Ctrl Pts',(0.435259874635114,-3.91056324675774,304.613611781005));
#7427=CARTESIAN_POINT('Ctrl Pts',(0.319595966757183,-3.91999329311066,304.607737677525));
#7428=CARTESIAN_POINT('Ctrl Pts',(0.204047588166283,-3.92941392039282,304.601869441312));
#7429=CARTESIAN_POINT('Ctrl Pts',(0.087963999044487,-3.93373090115052,304.596001205099));
#7430=CARTESIAN_POINT('Ctrl Pts',(-0.0281685801207231,-3.93289912546635,
304.590132968886));
#7431=CARTESIAN_POINT('Ctrl Pts',(-0.14653329841826,-3.93205136254529,304.584151941587));
#7432=CARTESIAN_POINT('Ctrl Pts',(-0.264948481105593,-3.92585479991437,
304.578170914289));
#7433=CARTESIAN_POINT('Ctrl Pts',(-0.382895478197291,-3.9143173163115,304.57218988699));
#7434=CARTESIAN_POINT('Ctrl Pts',(-0.498490903448139,-3.90300986163878,
304.566328106605));
#7435=CARTESIAN_POINT('Ctrl Pts',(-0.613636211076912,-3.8865725252648,304.56046632622));
#7436=CARTESIAN_POINT('Ctrl Pts',(-0.727845804985477,-3.86506526260101,
304.554604545835));
#7437=CARTESIAN_POINT('Ctrl Pts',(-0.84203960532356,-3.84356097408727,304.548743576051));
#7438=CARTESIAN_POINT('Ctrl Pts',(-0.955297544684902,-3.81698822974895,
304.542882606267));
#7439=CARTESIAN_POINT('Ctrl Pts',(-1.06714302021621,-3.78545833082387,304.537021636483));
#7440=CARTESIAN_POINT('Ctrl Pts',(-1.17899986089018,-3.75392522799806,304.531160071139));
#7441=CARTESIAN_POINT('Ctrl Pts',(-1.28944355605526,-3.71743408096652,304.525298505794));
#7442=CARTESIAN_POINT('Ctrl Pts',(-1.39801216409406,-3.67614621431807,304.51943694045));
#7443=CARTESIAN_POINT('Ctrl Pts',(-1.51045473897567,-3.63338510573259,304.513366221556));
#7444=CARTESIAN_POINT('Ctrl Pts',(-1.62088546638646,-3.58547873559274,304.507295502661));
#7445=CARTESIAN_POINT('Ctrl Pts',(-1.72881451684019,-3.53266038084085,304.501224783767));
#7446=CARTESIAN_POINT('Ctrl Pts',(-1.83317870755128,-3.48158659834023,304.495354578648));
#7447=CARTESIAN_POINT('Ctrl Pts',(-1.93520353332699,-3.42592044450438,304.489484373529));
#7448=CARTESIAN_POINT('Ctrl Pts',(-2.03447288800904,-3.3659187554004,304.48361416841));
#7449=CARTESIAN_POINT('Ctrl Pts',(-2.13882848909092,-3.3028427703451,304.477443192628));
#7450=CARTESIAN_POINT('Ctrl Pts',(-2.24013833713969,-3.2349754993727,304.471272216846));
#7451=CARTESIAN_POINT('Ctrl Pts',(-2.33795655125514,-3.16266472526621,304.465101241064));
#7452=CARTESIAN_POINT('Ctrl Pts',(-2.43577476537058,-3.09035395115972,304.458930265281));
#7453=CARTESIAN_POINT('Ctrl Pts',(-2.53010098584207,-3.01360005760262,304.452759289499));
#7454=CARTESIAN_POINT('Ctrl Pts',(-2.62053347657117,-2.93279615694132,304.446588313717));
#7455=CARTESIAN_POINT('Ctrl Pts',(-2.70672423362637,-2.85578236118208,304.440706787397));
#7456=CARTESIAN_POINT('Ctrl Pts',(-2.78965597749972,-2.77484175200591,304.434825261076));
#7457=CARTESIAN_POINT('Ctrl Pts',(-2.86895074997518,-2.69028076494198,304.428943734756));
#7458=CARTESIAN_POINT('Ctrl Pts',(-2.94814530867894,-2.60582664716071,304.423069641586));
#7459=CARTESIAN_POINT('Ctrl Pts',(-3.02371175836546,-2.51776154922697,304.417195548415));
#7460=CARTESIAN_POINT('Ctrl Pts',(-3.09530626831255,-2.42643114580757,304.411321455245));
#7461=CARTESIAN_POINT('Ctrl Pts',(-3.16682926478493,-2.33519196941801,304.405453229519));
#7462=CARTESIAN_POINT('Ctrl Pts',(-3.23438796115451,-2.24069429801477,304.399585003793));
#7463=CARTESIAN_POINT('Ctrl Pts',(-3.2976768286533,-2.14331904619053,304.393716778068));
#7464=CARTESIAN_POINT('Ctrl Pts',(-3.3621823038106,-2.04407194104044,304.387735746905));
#7465=CARTESIAN_POINT('Ctrl Pts',(-3.42225179757432,-1.94183579710125,304.381754715742));
#7466=CARTESIAN_POINT('Ctrl Pts',(-3.47760613315286,-1.83704778997651,304.375773684579));
#7467=CARTESIAN_POINT('Ctrl Pts',(-3.53185670443235,-1.73434925353234,304.369911915053));
#7468=CARTESIAN_POINT('Ctrl Pts',(-3.58157821540421,-1.62920005989815,304.364050145527));
#7469=CARTESIAN_POINT('Ctrl Pts',(-3.62655316235846,-1.52203848853696,304.358188376));
#7470=CARTESIAN_POINT('Ctrl Pts',(-3.67152188898382,-1.41489173832094,304.352327417195));
#7471=CARTESIAN_POINT('Ctrl Pts',(-3.71174519781089,-1.30573354350387,304.34646645839));
#7472=CARTESIAN_POINT('Ctrl Pts',(-3.74705338999338,-1.19502296736888,304.340605499585));
#7473=CARTESIAN_POINT('Ctrl Pts',(-3.78236516936451,-1.0843011434272,304.334743945327));
#7474=CARTESIAN_POINT('Ctrl Pts',(-3.81276071427995,-0.972027016978667,
304.328882391069));
#7475=CARTESIAN_POINT('Ctrl Pts',(-3.83812014989347,-0.858674976333749,
304.323020836812));
#7476=CARTESIAN_POINT('Ctrl Pts',(-3.86438458051746,-0.741277773455159,
304.316950102924));
#7477=CARTESIAN_POINT('Ctrl Pts',(-3.88524663614198,-0.622724749329648,
304.310879369036));
#7478=CARTESIAN_POINT('Ctrl Pts',(-3.90063112327204,-0.503553214825912,
304.304808635148));
#7479=CARTESIAN_POINT('Ctrl Pts',(-3.91550740077476,-0.388318381014748,
304.298938441283));
#7480=CARTESIAN_POINT('Ctrl Pts',(-3.92526231205771,-0.272505677092596,
304.293068247419));
#7481=CARTESIAN_POINT('Ctrl Pts',(-3.92988094354268,-0.156603861957868,
304.287198053554));
#7482=CARTESIAN_POINT('Ctrl Pts',(-3.93473625046463,-0.0347628172409708,
304.281027049654));
#7483=CARTESIAN_POINT('Ctrl Pts',(-3.93391493363068,0.087176183760976,304.274856045755));
#7484=CARTESIAN_POINT('Ctrl Pts',(-3.92746157474384,0.208649416271988,304.268685041856));
#7485=CARTESIAN_POINT('Ctrl Pts',(-3.921008215857,0.33012264878301,304.262514037956));
#7486=CARTESIAN_POINT('Ctrl Pts',(-3.90892293693869,0.451129601202003,304.256343034056));
#7487=CARTESIAN_POINT('Ctrl Pts',(-3.89131247210783,0.571118415407881,304.250172030157));
#7488=CARTESIAN_POINT('Ctrl Pts',(-3.87452808317339,0.685478765617703,304.244290497184));
#7489=CARTESIAN_POINT('Ctrl Pts',(-3.8526710536493,0.799282807439263,304.238408964212));
#7490=CARTESIAN_POINT('Ctrl Pts',(-3.82578888167082,0.912046288783581,304.232527431239));
#7491=CARTESIAN_POINT('Ctrl Pts',(-3.79894068327732,1.02466726007633,304.226653331325));
#7492=CARTESIAN_POINT('Ctrl Pts',(-3.76708006778264,1.13624988921146,304.220779231411));
#7493=CARTESIAN_POINT('Ctrl Pts',(-3.73030608239908,1.24631678622106,304.214905131497));
#7494=CARTESIAN_POINT('Ctrl Pts',(-3.69356882882083,1.35627374258135,304.209036898946));
#7495=CARTESIAN_POINT('Ctrl Pts',(-3.65192809787854,1.46471759014417,304.203168666394));
#7496=CARTESIAN_POINT('Ctrl Pts',(-3.60553344826318,1.57118348815644,304.197300433842));
#7497=CARTESIAN_POINT('Ctrl Pts',(-3.55824702506397,1.67969581773388,304.191319405207));
#7498=CARTESIAN_POINT('Ctrl Pts',(-3.50602214065162,1.78615295097963,304.185338376572));
#7499=CARTESIAN_POINT('Ctrl Pts',(-3.44906982329833,1.89008104429752,304.179357347937));
#7500=CARTESIAN_POINT('Ctrl Pts',(-3.39325304387148,1.99193697800772,304.173495571426));
#7501=CARTESIAN_POINT('Ctrl Pts',(-3.33289580730175,2.09136341065753,304.167633794916));
#7502=CARTESIAN_POINT('Ctrl Pts',(-3.26824404264322,2.18793735690195,304.161772018405));
#7503=CARTESIAN_POINT('Ctrl Pts',(-3.2036012192196,2.28449794712517,304.155911052569));
#7504=CARTESIAN_POINT('Ctrl Pts',(-3.13466527787735,2.378206493361,304.150050086733));
#7505=CARTESIAN_POINT('Ctrl Pts',(-3.06172583056679,2.46866845453983,304.144189120897));
#7506=CARTESIAN_POINT('Ctrl Pts',(-2.98877897238865,2.55913960692645,304.138327559569));
#7507=CARTESIAN_POINT('Ctrl Pts',(-2.91182805810292,2.64636319793497,304.132465998241));
#7508=CARTESIAN_POINT('Ctrl Pts',(-2.83120293942275,2.72997782331725,304.126604436913));
#7509=CARTESIAN_POINT('Ctrl Pts',(-2.74770080899298,2.81657613745064,304.12053371272));
#7510=CARTESIAN_POINT('Ctrl Pts',(-2.66025768582945,2.8993027666353,304.114462988527));
#7511=CARTESIAN_POINT('Ctrl Pts',(-2.56928054670307,2.97779893081,304.108392264334));
#7512=CARTESIAN_POINT('Ctrl Pts',(-2.48130849047592,3.05370227350359,304.102522063367));
#7513=CARTESIAN_POINT('Ctrl Pts',(-2.39003256385641,3.12565000216864,304.0966518624));
#7514=CARTESIAN_POINT('Ctrl Pts',(-2.29585243950112,3.19336038931354,304.090781661434));
#7515=CARTESIAN_POINT('Ctrl Pts',(-2.19684659388923,3.26454020758072,304.084610675627));
#7516=CARTESIAN_POINT('Ctrl Pts',(-2.09463149333541,3.33103665703813,304.078439689821));
#7517=CARTESIAN_POINT('Ctrl Pts',(-1.9897021452276,3.39257636218799,304.072268704015));
#7518=CARTESIAN_POINT('Ctrl Pts',(-1.8847727971198,3.45411606733785,304.066097718209));
#7519=CARTESIAN_POINT('Ctrl Pts',(-1.77712969562501,3.51069884814968,304.059926732403));
#7520=CARTESIAN_POINT('Ctrl Pts',(-1.66729218737832,3.56210973468073,304.053755746597));
#7521=CARTESIAN_POINT('Ctrl Pts',(-1.56260667784775,3.61110916063123,304.047874214835));
#7522=CARTESIAN_POINT('Ctrl Pts',(-1.45559066607334,3.65556877396117,304.041992683073));
#7523=CARTESIAN_POINT('Ctrl Pts',(-1.34667444822617,3.69526141571807,304.03611115131));
#7524=CARTESIAN_POINT('Ctrl Pts',(-1.2378958783929,3.73490389402446,304.030237052612));
#7525=CARTESIAN_POINT('Ctrl Pts',(-1.12722226223042,3.76979124274884,304.024362953913));
#7526=CARTESIAN_POINT('Ctrl Pts',(-1.01510657010295,3.79974310333394,304.018488855215));
#7527=CARTESIAN_POINT('Ctrl Pts',(-0.903102865156112,3.82966504639047,304.012620623882));
#7528=CARTESIAN_POINT('Ctrl Pts',(-0.789660345248424,3.85466120232958,304.006752392549));
#7529=CARTESIAN_POINT('Ctrl Pts',(-0.675249337169474,3.87460028037115,304.000884161216));
#7530=CARTESIAN_POINT('Ctrl Pts',(-0.558639147693519,3.89492262266533,303.994903132125));
#7531=CARTESIAN_POINT('Ctrl Pts',(-0.441023261496849,3.90999131716952,303.988922103034));
#7532=CARTESIAN_POINT('Ctrl Pts',(-0.322913385607228,3.91972141170717,303.982941073943));
#7533=CARTESIAN_POINT('Ctrl Pts',(-0.207158464222991,3.92925750104588,303.977079298651));
#7534=CARTESIAN_POINT('Ctrl Pts',(-0.0909294983870328,3.93366587280026,
303.97121752336));
#7535=CARTESIAN_POINT('Ctrl Pts',(0.0252850199611637,3.93291872122544,303.965355748068));
#7536=CARTESIAN_POINT('Ctrl Pts',(0.141483466069428,3.93217167298022,303.959494783448));
#7537=CARTESIAN_POINT('Ctrl Pts',(0.257667056973605,3.92627052199346,303.953633818828));
#7538=CARTESIAN_POINT('Ctrl Pts',(0.373346971566622,3.91523958894242,303.947772854208));
#7539=CARTESIAN_POINT('Ctrl Pts',(0.489038639661692,3.90420753510828,303.941911294093));
#7540=CARTESIAN_POINT('Ctrl Pts',(0.604226119765026,3.88804470218821,303.936049733978));
#7541=CARTESIAN_POINT('Ctrl Pts',(0.718426074707708,3.86682724920316,303.930188173863));
#7542=CARTESIAN_POINT('Ctrl Pts',(0.836701177391101,3.84485266583536,303.924117447961));
#7543=CARTESIAN_POINT('Ctrl Pts',(0.953916490991689,3.81745606708269,303.918046722058));
#7544=CARTESIAN_POINT('Ctrl Pts',(1.06954837564919,3.78477942186149,303.911975996156));
#7545=CARTESIAN_POINT('Ctrl Pts',(1.18136074770322,3.75318214033509,303.906105796382));
#7546=CARTESIAN_POINT('Ctrl Pts',(1.2916922678671,3.71664831157857,303.900235596608));
#7547=CARTESIAN_POINT('Ctrl Pts',(1.40008762461898,3.67535626074382,303.894365396833));
#7548=CARTESIAN_POINT('Ctrl Pts',(1.51403716232148,3.63194840413075,303.888194407867));
#7549=CARTESIAN_POINT('Ctrl Pts',(1.62584637718348,3.58328199783037,303.882023418901));
#7550=CARTESIAN_POINT('Ctrl Pts',(1.73501440219909,3.52961952966063,303.875852429935));
#7551=CARTESIAN_POINT('Ctrl Pts',(1.8441824272147,3.47595706149089,303.869681440968));
#7552=CARTESIAN_POINT('Ctrl Pts',(1.95070883987929,3.41729884466744,303.863510452002));
#7553=CARTESIAN_POINT('Ctrl Pts',(2.0541281053617,3.3539598576553,303.857339463036));
#7554=CARTESIAN_POINT('Ctrl Pts',(2.15269635933167,3.29359186597704,303.851457932116));
#7555=CARTESIAN_POINT('Ctrl Pts',(2.24875994985064,3.22877777680599,303.845576401196));
#7556=CARTESIAN_POINT('Ctrl Pts',(2.3418922328573,3.15975153606777,303.839694870276));
#7557=CARTESIAN_POINT('Ctrl Pts',(2.43490681524703,3.09081253072051,303.833820772437));
#7558=CARTESIAN_POINT('Ctrl Pts',(2.52499712999191,3.01767220416633,303.827946674598));
#7559=CARTESIAN_POINT('Ctrl Pts',(2.61176309746407,2.94060920945387,303.822072576759));
#7560=CARTESIAN_POINT('Ctrl Pts',(2.69844239816774,2.86362318963049,303.816204346302));
#7561=CARTESIAN_POINT('Ctrl Pts',(2.78180365085279,2.78272256786997,303.810336115845));
#7562=CARTESIAN_POINT('Ctrl Pts',(2.86147816236328,2.69822751566988,303.804467885388));
#7563=CARTESIAN_POINT('Ctrl Pts',(2.94268417502951,2.61210830202036,303.798486855975));
#7564=CARTESIAN_POINT('Ctrl Pts',(3.02005989973372,2.52225530454719,303.792505826562));
#7565=CARTESIAN_POINT('Ctrl Pts',(3.09325251609353,2.42904875860511,303.786524797149));
#7566=CARTESIAN_POINT('Ctrl Pts',(3.16498575360255,2.3377006468695,303.780663022768));
#7567=CARTESIAN_POINT('Ctrl Pts',(3.23270088527501,2.24313181847449,303.774801248388));
#7568=CARTESIAN_POINT('Ctrl Pts',(3.2961055721996,2.14573461940539,303.768939474007));
#7569=CARTESIAN_POINT('Ctrl Pts',(3.35950149025488,2.0483508903706,303.76307851031));
#7570=CARTESIAN_POINT('Ctrl Pts',(3.41858792448416,1.94813991359881,303.757217546613));
#7571=CARTESIAN_POINT('Ctrl Pts',(3.47311585615841,1.84552302876476,303.751356582916));
#7572=CARTESIAN_POINT('Ctrl Pts',(3.52764932797323,1.7428957178619,303.745495023734));
#7573=CARTESIAN_POINT('Ctrl Pts',(3.57762318328595,1.63786237661532,303.739633464551));
#7574=CARTESIAN_POINT('Ctrl Pts',(3.62283468586133,1.53086832840712,303.733771905369));
#7575=CARTESIAN_POINT('Ctrl Pts',(3.66965954730188,1.42005622978335,303.727701178212));
#7576=CARTESIAN_POINT('Ctrl Pts',(3.71137563286428,1.30714131382758,303.721630451054));
#7577=CARTESIAN_POINT('Ctrl Pts',(3.74781292236082,1.19263879652864,303.715559723896));
#7578=CARTESIAN_POINT('Ctrl Pts',(3.78304661486231,1.08191852779017,303.709689525072));
#7579=CARTESIAN_POINT('Ctrl Pts',(3.81334469335758,0.969714304700055,303.703819326249));
#7580=CARTESIAN_POINT('Ctrl Pts',(3.83860512395872,0.856504350437184,303.697949127425));
#7581=CARTESIAN_POINT('Ctrl Pts',(3.86515991414326,0.737493450357144,303.6917781361));
#7582=CARTESIAN_POINT('Ctrl Pts',(3.88614702616928,0.617371542182774,303.685607144776));
#7583=CARTESIAN_POINT('Ctrl Pts',(3.90150956439052,0.496701237132804,303.679436153451));
#7584=CARTESIAN_POINT('Ctrl Pts',(3.91687210261177,0.376030932082834,303.673265162126));
#7585=CARTESIAN_POINT('Ctrl Pts',(3.92661009564078,0.254812755321279,303.667094170801));
#7586=CARTESIAN_POINT('Ctrl Pts',(3.93072991968281,0.13360875162347,303.660923179476));
#7587=CARTESIAN_POINT('Ctrl Pts',(3.93223419442983,0.0893534338866097,303.658669960329));
#7588=CARTESIAN_POINT('Ctrl Pts',(3.93299110200493,0.0450725701889574,303.656416741182));
#7589=CARTESIAN_POINT('Ctrl Pts',(3.93299992201098,0.000783237888672866,
303.654163522035));
#7590=CARTESIAN_POINT('',(3.93299951520447,0.0019527932382245,302.404163522072));
#7591=CARTESIAN_POINT('Ctrl Pts',(3.93299992201116,0.00078323698981516,
303.654163521989));
#7592=CARTESIAN_POINT('Ctrl Pts',(3.93302281745676,-0.114185523302119,303.648314487955));
#7593=CARTESIAN_POINT('Ctrl Pts',(3.92800032631236,-0.229348643469013,303.64246545392));
#7594=CARTESIAN_POINT('Ctrl Pts',(3.91790739951338,-0.344224648795359,303.636616419885));
#7595=CARTESIAN_POINT('Ctrl Pts',(3.90782710347176,-0.458956892953262,303.630774705603));
#7596=CARTESIAN_POINT('Ctrl Pts',(3.8926890250553,-0.573402325072434,303.624932991321));
#7597=CARTESIAN_POINT('Ctrl Pts',(3.87252011576164,-0.687078563936791,303.619091277039));
#7598=CARTESIAN_POINT('Ctrl Pts',(3.85237094282903,-0.800643564495698,303.613255279188));
#7599=CARTESIAN_POINT('Ctrl Pts',(3.82720080237384,-0.913440460580957,303.607419281338));
#7600=CARTESIAN_POINT('Ctrl Pts',(3.79708846201241,-1.02499181052936,303.601583283487));
#7601=CARTESIAN_POINT('Ctrl Pts',(3.76699639105037,-1.13646807236309,303.595751213998));
#7602=CARTESIAN_POINT('Ctrl Pts',(3.73196884489983,-1.2467000542881,303.589919144509));
#7603=CARTESIAN_POINT('Ctrl Pts',(3.69213556805134,-1.35522099567937,303.58408707502));
#7604=CARTESIAN_POINT('Ctrl Pts',(3.65231622209874,-1.46370398403098,303.578257045182));
#7605=CARTESIAN_POINT('Ctrl Pts',(3.6076946297648,-1.57047673042795,303.572427015343));
#7606=CARTESIAN_POINT('Ctrl Pts',(3.55845004246602,-1.67508874250696,303.566596985505));
#7607=CARTESIAN_POINT('Ctrl Pts',(3.50921051334932,-1.77969000931156,303.5607675545));
#7608=CARTESIAN_POINT('Ctrl Pts',(3.45534911114047,-1.88213060601439,303.554938123496));
#7609=CARTESIAN_POINT('Ctrl Pts',(3.39709245674577,-1.98198179616287,303.549108692492));
#7610=CARTESIAN_POINT('Ctrl Pts',(3.33882739578794,-2.08184739505731,303.543278420288));
#7611=CARTESIAN_POINT('Ctrl Pts',(3.2761660323174,-2.17912248475528,303.537448148084));
#7612=CARTESIAN_POINT('Ctrl Pts',(3.20937959701542,-2.27340528772613,303.53161787588));
#7613=CARTESIAN_POINT('Ctrl Pts',(3.14252613685886,-2.36778271007785,303.525781752591));
#7614=CARTESIAN_POINT('Ctrl Pts',(3.07153957837072,-2.45916150746637,303.519945629302));
#7615=CARTESIAN_POINT('Ctrl Pts',(2.99673300382066,-2.54717103937133,303.514109506012));
#7616=CARTESIAN_POINT('Ctrl Pts',(2.92188788897986,-2.63522591372069,303.508270375956));
#7617=CARTESIAN_POINT('Ctrl Pts',(2.84321912185116,-2.71990775983271,303.502431245901));
#7618=CARTESIAN_POINT('Ctrl Pts',(2.76107712497651,-2.8008823805957,303.496592115845));
#7619=CARTESIAN_POINT('Ctrl Pts',(2.67880484893882,-2.88198542903542,303.49074372479));
#7620=CARTESIAN_POINT('Ctrl Pts',(2.59304864821594,-2.95936922681172,303.484895333735));
#7621=CARTESIAN_POINT('Ctrl Pts',(2.50419283663215,-3.03273922996361,303.47904694268));
#7622=CARTESIAN_POINT('Ctrl Pts',(2.43055619346647,-3.09354246438193,303.474200260425));
#7623=CARTESIAN_POINT('Ctrl Pts',(2.35479148636737,-3.15158980484418,303.469353578171));
#7624=CARTESIAN_POINT('Ctrl Pts',(2.27713161213407,-3.20673675580327,303.464506895916));
#7625=CARTESIAN_POINT('Ctrl Pts',(2.18289003236076,-3.2736585198336,303.458625364471));
#7626=CARTESIAN_POINT('Ctrl Pts',(2.08554403724773,-3.33653013104214,303.452743833026));
#7627=CARTESIAN_POINT('Ctrl Pts',(1.98547639138384,-3.39505117770814,303.446862301581));
#7628=CARTESIAN_POINT('Ctrl Pts',(1.88553521088994,-3.45349826554603,303.440988203208));
#7629=CARTESIAN_POINT('Ctrl Pts',(1.7828795729352,-3.50760551789798,303.435114104835));
#7630=CARTESIAN_POINT('Ctrl Pts',(1.67792291624083,-3.5571145170143,303.429240006462));
#7631=CARTESIAN_POINT('Ctrl Pts',(1.57307109605297,-3.60657406380742,303.423371775464));
#7632=CARTESIAN_POINT('Ctrl Pts',(1.4659231995758,-3.65144431930907,303.417503544465));
#7633=CARTESIAN_POINT('Ctrl Pts',(1.35691851279986,-3.6915120411047,303.411635313466));
#7634=CARTESIAN_POINT('Ctrl Pts',(1.24581855506428,-3.73234993835224,303.405654284253));
#7635=CARTESIAN_POINT('Ctrl Pts',(1.13279006261976,-3.76819854734679,303.39967325504));
#7636=CARTESIAN_POINT('Ctrl Pts',(1.0183213179728,-3.7988828217467,303.393692225827));
#7637=CARTESIAN_POINT('Ctrl Pts',(0.906134937536904,-3.82895528992868,303.387830450888));
#7638=CARTESIAN_POINT('Ctrl Pts',(0.792565622138403,-3.85406734576113,303.381968675949));
#7639=CARTESIAN_POINT('Ctrl Pts',(0.678089027243571,-3.87410431856602,303.37610690101));
#7640=CARTESIAN_POINT('Ctrl Pts',(0.563628264361583,-3.89413852027511,303.370245936749));
#7641=CARTESIAN_POINT('Ctrl Pts',(0.448260877050694,-3.90909896380373,303.364384972489));
#7642=CARTESIAN_POINT('Ctrl Pts',(0.332472161685852,-3.918922206641,303.358524008228));
#7643=CARTESIAN_POINT('Ctrl Pts',(0.21667168188089,-3.92874644754575,303.352662448478));
#7644=CARTESIAN_POINT('Ctrl Pts',(0.100450199256683,-3.93343241534604,303.346800888727));
#7645=CARTESIAN_POINT('Ctrl Pts',(-0.0157031198889865,-3.93296865128947,
303.340939328977));
#7646=CARTESIAN_POINT('Ctrl Pts',(-0.136001308306843,-3.93248833805979,
303.334868602592));
#7647=CARTESIAN_POINT('Ctrl Pts',(-0.256225900974122,-3.92648389608309,
303.328797876207));
#7648=CARTESIAN_POINT('Ctrl Pts',(-0.375836314876531,-3.91500141308021,
303.322727149822));
#7649=CARTESIAN_POINT('Ctrl Pts',(-0.491495782150235,-3.90389821709783,
303.316856950424));
#7650=CARTESIAN_POINT('Ctrl Pts',(-0.606580599238758,-3.88767328386376,
303.310986751026));
#7651=CARTESIAN_POINT('Ctrl Pts',(-0.720610913079052,-3.8664206848132,303.305116551628));
#7652=CARTESIAN_POINT('Ctrl Pts',(-0.840484168634247,-3.8440790972879,303.29894556175));
#7653=CARTESIAN_POINT('Ctrl Pts',(-0.959191476892085,-3.81618107976753,
303.292774571871));
#7654=CARTESIAN_POINT('Ctrl Pts',(-1.07619311940163,-3.78289536859699,303.286603581992));
#7655=CARTESIAN_POINT('Ctrl Pts',(-1.19319476191117,-3.74960965742646,303.280432592113));
#7656=CARTESIAN_POINT('Ctrl Pts',(-1.3084902669871,-3.71093648525967,303.274261602235));
#7657=CARTESIAN_POINT('Ctrl Pts',(-1.42156529726405,-3.66710254909984,303.268090612356));
#7658=CARTESIAN_POINT('Ctrl Pts',(-1.5293363926921,-3.62532470207829,303.262209080974));
#7659=CARTESIAN_POINT('Ctrl Pts',(-1.63543784988199,-3.57872467305038,303.256327549592));
#7660=CARTESIAN_POINT('Ctrl Pts',(-1.73940807988741,-3.5274563826676,303.25044601821));
#7661=CARTESIAN_POINT('Ctrl Pts',(-1.84324691241313,-3.47625288510239,303.244571919901));
#7662=CARTESIAN_POINT('Ctrl Pts',(-1.94495950844133,-3.42039304042524,303.238697821593));
#7663=CARTESIAN_POINT('Ctrl Pts',(-2.04410242477204,-3.36007950457144,303.232823723285));
#7664=CARTESIAN_POINT('Ctrl Pts',(-2.14314631165635,-3.29982621322413,303.226955492352));
#7665=CARTESIAN_POINT('Ctrl Pts',(-2.23962527490243,-3.23512829294086,303.221087261419));
#7666=CARTESIAN_POINT('Ctrl Pts',(-2.3331193313831,-3.16623485950213,303.215219030486));
#7667=CARTESIAN_POINT('Ctrl Pts',(-2.42841051738148,-3.0960171662391,303.209238001249));
#7668=CARTESIAN_POINT('Ctrl Pts',(-2.52060047000611,-3.02144119402228,303.203256972012));
#7669=CARTESIAN_POINT('Ctrl Pts',(-2.60927408767226,-2.94281799223161,303.197275942775));
#7670=CARTESIAN_POINT('Ctrl Pts',(-2.69617966245841,-2.865762440389,303.191414167905));
#7671=CARTESIAN_POINT('Ctrl Pts',(-2.77970750465655,-2.78481984324435,303.185552393035));
#7672=CARTESIAN_POINT('Ctrl Pts',(-2.85949985540938,-2.70032397628762,303.179690618165));
#7673=CARTESIAN_POINT('Ctrl Pts',(-2.9392811709355,-2.61583979505061,303.173829653975));
#7674=CARTESIAN_POINT('Ctrl Pts',(-3.01532773974606,-2.52780362060482,303.167968689784));
#7675=CARTESIAN_POINT('Ctrl Pts',(-3.08731924325342,-2.43658549824075,303.162107725594));
#7676=CARTESIAN_POINT('Ctrl Pts',(-3.15931806127636,-2.34535810788888,303.156246165914));
#7677=CARTESIAN_POINT('Ctrl Pts',(-3.22726073983907,-2.25094845019649,303.150384606235));
#7678=CARTESIAN_POINT('Ctrl Pts',(-3.29086821071063,-2.1537584404325,303.144523046556));
#7679=CARTESIAN_POINT('Ctrl Pts',(-3.35674548210072,-2.05310025418646,303.138452320076));
#7680=CARTESIAN_POINT('Ctrl Pts',(-3.41797210375618,-1.94945997573294,303.132381593596));
#7681=CARTESIAN_POINT('Ctrl Pts',(-3.47428870424946,-1.84331413479217,303.126310867116));
#7682=CARTESIAN_POINT('Ctrl Pts',(-3.52874506483207,-1.74067448435188,303.120440667791));
#7683=CARTESIAN_POINT('Ctrl Pts',(-3.57861053220966,-1.63569258845348,303.114570468466));
#7684=CARTESIAN_POINT('Ctrl Pts',(-3.62369923834598,-1.52882073180958,303.108700269142));
#7685=CARTESIAN_POINT('Ctrl Pts',(-3.67109830299077,-1.4164727299295,303.102529279084));
#7686=CARTESIAN_POINT('Ctrl Pts',(-3.713217931585,-1.30203644971664,303.096358289026));
#7687=CARTESIAN_POINT('Ctrl Pts',(-3.74990158412267,-1.18605527248703,303.090187298969));
#7688=CARTESIAN_POINT('Ctrl Pts',(-3.78658523666034,-1.07007409525744,303.084016308911));
#7689=CARTESIAN_POINT('Ctrl Pts',(-3.81783284742591,-0.952548542831441,
303.077845318853));
#7690=CARTESIAN_POINT('Ctrl Pts',(-3.84355023053837,-0.834032748354919,
303.071674328796));
#7691=CARTESIAN_POINT('Ctrl Pts',(-3.86806130514394,-0.721076096908286,
303.065792797342));
#7692=CARTESIAN_POINT('Ctrl Pts',(-3.88762819483243,-0.606856050001968,
303.059911265888));
#7693=CARTESIAN_POINT('Ctrl Pts',(-3.90212504068358,-0.491842624088376,
303.054029734433));
#7694=CARTESIAN_POINT('Ctrl Pts',(-3.91660356543746,-0.376974552011518,
303.048155636052));
#7695=CARTESIAN_POINT('Ctrl Pts',(-3.92602473886699,-0.261315500137586,
303.042281537671));
#7696=CARTESIAN_POINT('Ctrl Pts',(-3.93031337093058,-0.14534719221326,303.036407439289));
#7697=CARTESIAN_POINT('Ctrl Pts',(-3.93459771927125,-0.029494719849412,
303.030539208283));
#7698=CARTESIAN_POINT('Ctrl Pts',(-3.93375970938358,0.0866659848548804,
303.024670977276));
#7699=CARTESIAN_POINT('Ctrl Pts',(-3.927775849082,0.202647179521869,303.018802746269));
#7700=CARTESIAN_POINT('Ctrl Pts',(-3.92167696796974,0.320857746260009,303.012821717059));
#7701=CARTESIAN_POINT('Ctrl Pts',(-3.91023231220583,0.438881399424562,303.006840687849));
#7702=CARTESIAN_POINT('Ctrl Pts',(-3.89347276509992,0.556200348278578,303.000859658639));
#7703=CARTESIAN_POINT('Ctrl Pts',(-3.87704738246301,0.671180103597108,302.994997883693));
#7704=CARTESIAN_POINT('Ctrl Pts',(-3.8555171511324,0.785482570408821,302.989136108747));
#7705=CARTESIAN_POINT('Ctrl Pts',(-3.82896351313979,0.898625291789752,302.983274333801));
#7706=CARTESIAN_POINT('Ctrl Pts',(-3.80241354749404,1.01175236562296,302.977413369534));
#7707=CARTESIAN_POINT('Ctrl Pts',(-3.77084165086854,1.12371961218863,302.971552405267));
#7708=CARTESIAN_POINT('Ctrl Pts',(-3.73438016152757,1.23405583714405,302.965691440999));
#7709=CARTESIAN_POINT('Ctrl Pts',(-3.69791496760562,1.34440327254336,302.959829881243));
#7710=CARTESIAN_POINT('Ctrl Pts',(-3.65655932259171,1.45311896589117,302.953968321487));
#7711=CARTESIAN_POINT('Ctrl Pts',(-3.61049488832033,1.55974858916838,302.948106761731));
#7712=CARTESIAN_POINT('Ctrl Pts',(-3.56278666940059,1.6701832334032,302.942036035356));
#7713=CARTESIAN_POINT('Ctrl Pts',(-3.51002750913876,1.77837970737051,302.935965308981));
#7714=CARTESIAN_POINT('Ctrl Pts',(-3.45247218995707,1.88385901212724,302.929894582607));
#7715=CARTESIAN_POINT('Ctrl Pts',(-3.39681802611691,1.98585414641094,302.924024383204));
#7716=CARTESIAN_POINT('Ctrl Pts',(-3.33667982061495,2.08530845684434,302.918154183801));
#7717=CARTESIAN_POINT('Ctrl Pts',(-3.27233261907056,2.18181764365558,302.912283984399));
#7718=CARTESIAN_POINT('Ctrl Pts',(-3.20468825112871,2.28327198488167,302.906112994538));
#7719=CARTESIAN_POINT('Ctrl Pts',(-3.13239243580357,2.3814709637078,302.899942004677));
#7720=CARTESIAN_POINT('Ctrl Pts',(-3.05581240058875,2.47598456627016,302.893771014817));
#7721=CARTESIAN_POINT('Ctrl Pts',(-2.97923236537393,2.5704981688325,302.887600024956));
#7722=CARTESIAN_POINT('Ctrl Pts',(-2.89836850954299,2.6613260527928,302.881429035095));
#7723=CARTESIAN_POINT('Ctrl Pts',(-2.8136313873192,2.74808431753689,302.875258045235));
#7724=CARTESIAN_POINT('Ctrl Pts',(-2.73286897173148,2.83077307128554,302.869376513804));
#7725=CARTESIAN_POINT('Ctrl Pts',(-2.64832821169403,2.9100317746915,302.863494982373));
#7726=CARTESIAN_POINT('Ctrl Pts',(-2.56033201258136,2.98549643867667,302.857613450943));
#7727=CARTESIAN_POINT('Ctrl Pts',(-2.47244702296915,3.06086573050181,302.851739352585));
#7728=CARTESIAN_POINT('Ctrl Pts',(-2.38111558943836,3.13245025346504,302.845865254227));
#7729=CARTESIAN_POINT('Ctrl Pts',(-2.28669830350421,3.19992185353814,302.83999115587));
#7730=CARTESIAN_POINT('Ctrl Pts',(-2.19237532678118,3.26732605924258,302.834122924886));
#7731=CARTESIAN_POINT('Ctrl Pts',(-2.09497296236576,3.3306252762734,302.828254693903));
#7732=CARTESIAN_POINT('Ctrl Pts',(-1.99488530741481,3.38953117853495,302.82238646292));
#7733=CARTESIAN_POINT('Ctrl Pts',(-1.89287378292001,3.44956936100997,302.816405433702));
#7734=CARTESIAN_POINT('Ctrl Pts',(-1.78807299843604,3.50504330508081,302.810424404483));
#7735=CARTESIAN_POINT('Ctrl Pts',(-1.68093208576082,3.55569350803184,302.804443375264));
#7736=CARTESIAN_POINT('Ctrl Pts',(-1.57592742985989,3.60533380882251,302.798581600343));
#7737=CARTESIAN_POINT('Ctrl Pts',(-1.46867548891796,3.65034076207152,302.792719825421));
#7738=CARTESIAN_POINT('Ctrl Pts',(-1.35962376252657,3.69051652541661,302.786858050499));
#7739=CARTESIAN_POINT('Ctrl Pts',(-1.25058711790335,3.73068673248516,302.780997086256));
#7740=CARTESIAN_POINT('Ctrl Pts',(-1.13975156915167,3.76602693607683,302.775136122013));
#7741=CARTESIAN_POINT('Ctrl Pts',(-1.02758325800181,3.79638797383439,302.76927515777));
#7742=CARTESIAN_POINT('Ctrl Pts',(-0.915403550264176,3.82675209635117,302.763413598038));
#7743=CARTESIAN_POINT('Ctrl Pts',(-0.801891208443604,3.85213593975903,302.757552038306));
#7744=CARTESIAN_POINT('Ctrl Pts',(-0.687525473410276,3.87244079663098,302.751690478574));
#7745=CARTESIAN_POINT('Ctrl Pts',(-0.569078657271046,3.8934702216414,302.745619752166));
#7746=CARTESIAN_POINT('Ctrl Pts',(-0.449716873294232,3.90905132129786,302.739549025757));
#7747=CARTESIAN_POINT('Ctrl Pts',(-0.329980236899369,3.91913281776158,302.733478299349));
#7748=CARTESIAN_POINT('Ctrl Pts',(-0.21419871731156,3.92888130423517,302.727608099971));
#7749=CARTESIAN_POINT('Ctrl Pts',(-0.0980671387366002,3.93348781893119,
302.721737900592));
#7750=CARTESIAN_POINT('Ctrl Pts',(0.0179255588310843,3.93295914984387,302.715867701214));
#7751=CARTESIAN_POINT('Ctrl Pts',(0.139861752424025,3.93240339161486,302.709696711291));
#7752=CARTESIAN_POINT('Ctrl Pts',(0.261643926491458,3.92617228084734,302.703525721368));
#7753=CARTESIAN_POINT('Ctrl Pts',(0.38271089412944,3.91433536778782,302.697354731444));
#7754=CARTESIAN_POINT('Ctrl Pts',(0.503777861767422,3.90249845472831,302.691183741521));
#7755=CARTESIAN_POINT('Ctrl Pts',(0.62412911730201,3.88505588397551,302.685012751598));
#7756=CARTESIAN_POINT('Ctrl Pts',(0.743218086348091,3.86213876966184,302.678841761675));
#7757=CARTESIAN_POINT('Ctrl Pts',(0.856721028788252,3.84029661309877,302.672960230248));
#7758=CARTESIAN_POINT('Ctrl Pts',(0.969443132990848,3.81341149870362,302.667078698821));
#7759=CARTESIAN_POINT('Ctrl Pts',(1.08090273155214,3.7815523644296,302.661197167394));
#7760=CARTESIAN_POINT('Ctrl Pts',(1.19222146759259,3.74973349369523,302.655323069041));
#7761=CARTESIAN_POINT('Ctrl Pts',(1.30228047876846,3.71295321749396,302.649448970687));
#7762=CARTESIAN_POINT('Ctrl Pts',(1.41060724030692,3.67133166760968,302.643574872333));
#7763=CARTESIAN_POINT('Ctrl Pts',(1.51882579907799,3.62975169163398,302.637706641354));
#7764=CARTESIAN_POINT('Ctrl Pts',(1.6253151679036,3.58334020837525,302.631838410375));
#7765=CARTESIAN_POINT('Ctrl Pts',(1.72961760009881,3.5322672545305,302.625970179396));
#7766=CARTESIAN_POINT('Ctrl Pts',(1.83592491773799,3.48021258415634,302.619989150176));
#7767=CARTESIAN_POINT('Ctrl Pts',(1.93995993808236,3.4233155064749,302.614008120956));
#7768=CARTESIAN_POINT('Ctrl Pts',(2.04125864743232,3.36180786694938,302.608027091735));
#7769=CARTESIAN_POINT('Ctrl Pts',(2.14053758619138,3.30152661344821,302.602165316818));
#7770=CARTESIAN_POINT('Ctrl Pts',(2.23718795307342,3.23681717642422,302.5963035419));
#7771=CARTESIAN_POINT('Ctrl Pts',(2.33079809162539,3.16794401088078,302.590441766983));
#7772=CARTESIAN_POINT('Ctrl Pts',(2.4243952839673,3.0990803704431,302.584580802744));
#7773=CARTESIAN_POINT('Ctrl Pts',(2.51495275253663,3.02605439064325,302.578719838506));
#7774=CARTESIAN_POINT('Ctrl Pts',(2.60208919539501,2.94917290425783,302.572858874267));
#7775=CARTESIAN_POINT('Ctrl Pts',(2.68923449153811,2.87228360651741,302.566997314539));
#7776=CARTESIAN_POINT('Ctrl Pts',(2.77295776220374,2.79153829591852,302.561135754812));
#7777=CARTESIAN_POINT('Ctrl Pts',(2.85291259512011,2.70728253505337,302.555274195084));
#7778=CARTESIAN_POINT('Ctrl Pts',(2.93572057434127,2.62002015152389,302.54920346867));
#7779=CARTESIAN_POINT('Ctrl Pts',(3.01448581251738,2.52899244459729,302.543132742256));
#7780=CARTESIAN_POINT('Ctrl Pts',(3.08886794048322,2.43462191032919,302.537062015842));
#7781=CARTESIAN_POINT('Ctrl Pts',(3.16079309263549,2.34336860497818,302.531191816468));
#7782=CARTESIAN_POINT('Ctrl Pts',(3.22861993213251,2.24899019988977,302.525321617094));
#7783=CARTESIAN_POINT('Ctrl Pts',(3.29208474305134,2.15189847450305,302.51945141772));
#7784=CARTESIAN_POINT('Ctrl Pts',(3.35880150757975,2.04983174356193,302.513280427786));
#7785=CARTESIAN_POINT('Ctrl Pts',(3.42069711094658,1.94476672081367,302.507109437852));
#7786=CARTESIAN_POINT('Ctrl Pts',(3.47752041045996,1.83721005735175,302.500938447918));
#7787=CARTESIAN_POINT('Ctrl Pts',(3.53434370997332,1.72965339388984,302.494767457983));
#7788=CARTESIAN_POINT('Ctrl Pts',(3.5860945477062,1.61960559138547,302.488596468049));
#7789=CARTESIAN_POINT('Ctrl Pts',(3.6325812091907,1.5075950247446,302.482425478115));
#7790=CARTESIAN_POINT('Ctrl Pts',(3.68173078294175,1.38916811624636,302.475900993129));
#7791=CARTESIAN_POINT('Ctrl Pts',(3.72513134234822,1.26822460025763,302.469376508143));
#7792=CARTESIAN_POINT('Ctrl Pts',(3.76254653351109,1.14530894660074,302.462852023158));
#7793=CARTESIAN_POINT('Ctrl Pts',(3.79986192435122,1.02272115501065,302.456344941416));
#7794=CARTESIAN_POINT('Ctrl Pts',(3.83122370243373,0.898171951789454,302.449837859675));
#7795=CARTESIAN_POINT('Ctrl Pts',(3.85644381831002,0.772224110099149,302.443330777933));
#7796=CARTESIAN_POINT('Ctrl Pts',(3.88174452838295,0.645873785519059,302.436802901956));
#7797=CARTESIAN_POINT('Ctrl Pts',(3.90086408695092,0.518116083530064,302.430275025979));
#7798=CARTESIAN_POINT('Ctrl Pts',(3.91366178017579,0.38953879189533,302.423747150002));
#7799=CARTESIAN_POINT('Ctrl Pts',(3.92645947340065,0.260961500260597,302.417219274026));
#7800=CARTESIAN_POINT('Ctrl Pts',(3.93293516086949,0.131564860360707,302.410691398049));
#7801=CARTESIAN_POINT('Ctrl Pts',(3.93299951520447,0.00195279323822586,
302.404163522072));
#7802=CARTESIAN_POINT('',(3.93299852553402,-0.00340560526560608,301.154163522075));
#7803=CARTESIAN_POINT('Ctrl Pts',(3.93299951520483,0.00195279250481771,
302.404163522035));
#7804=CARTESIAN_POINT('Ctrl Pts',(3.93305803804962,-0.115914476855165,302.398227169555));
#7805=CARTESIAN_POINT('Ctrl Pts',(3.92781370480953,-0.233779881318091,302.392290817075));
#7806=CARTESIAN_POINT('Ctrl Pts',(3.91729349463852,-0.351141961125049,302.386354464595));
#7807=CARTESIAN_POINT('Ctrl Pts',(3.90677049323188,-0.46853517958927,302.380416537074));
#7808=CARTESIAN_POINT('Ctrl Pts',(3.89096886348083,-0.585424412293054,302.374478609553));
#7809=CARTESIAN_POINT('Ctrl Pts',(3.86996741386578,-0.701313920877823,302.368540682032));
#7810=CARTESIAN_POINT('Ctrl Pts',(3.84895588624024,-0.817259041608628,302.362599905066));
#7811=CARTESIAN_POINT('Ctrl Pts',(3.82273964196988,-0.932203092995342,302.356659128099));
#7812=CARTESIAN_POINT('Ctrl Pts',(3.79144837889095,-1.04566160405993,302.350718351132));
#7813=CARTESIAN_POINT('Ctrl Pts',(3.76011406092106,-1.15927622719358,302.344769400015));
#7814=CARTESIAN_POINT('Ctrl Pts',(3.72369088340339,-1.27140084469433,302.338820448897));
#7815=CARTESIAN_POINT('Ctrl Pts',(3.68235826933376,-1.38156671075605,302.33287149778));
#7816=CARTESIAN_POINT('Ctrl Pts',(3.64099469302163,-1.49181510201818,302.326918090305));
#7817=CARTESIAN_POINT('Ctrl Pts',(3.59471450688456,-1.60010145340699,302.320964682831));
#7818=CARTESIAN_POINT('Ctrl Pts',(3.54374435715108,-1.70597917078722,302.315011275357));
#7819=CARTESIAN_POINT('Ctrl Pts',(3.49268548173506,-1.81204119354598,302.30904750456));
#7820=CARTESIAN_POINT('Ctrl Pts',(3.4369205206017,-1.91568585680902,302.303083733762));
#7821=CARTESIAN_POINT('Ctrl Pts',(3.37672123785625,-2.0164926684247,302.297119962965));
#7822=CARTESIAN_POINT('Ctrl Pts',(3.33933659695329,-2.0790951826234,302.293416373495));
#7823=CARTESIAN_POINT('Ctrl Pts',(3.30024267610691,-2.14060383582257,302.289712784024));
#7824=CARTESIAN_POINT('Ctrl Pts',(3.25951245570129,-2.2009242492935,302.286009194554));
#7825=CARTESIAN_POINT('Ctrl Pts',(3.1948303213986,-2.29671683392635,302.280127663123));
#7826=CARTESIAN_POINT('Ctrl Pts',(3.12581760277882,-2.38980994238612,302.274246131692));
#7827=CARTESIAN_POINT('Ctrl Pts',(3.0527269461845,-2.47978773124617,302.268364600261));
#7828=CARTESIAN_POINT('Ctrl Pts',(2.97972866148272,-2.56965180627423,302.262490501903));
#7829=CARTESIAN_POINT('Ctrl Pts',(2.90266294612185,-2.65640807518571,302.256616403544));
#7830=CARTESIAN_POINT('Ctrl Pts',(2.82182593083435,-2.73966921654255,302.250742305186));
#7831=CARTESIAN_POINT('Ctrl Pts',(2.74106966003267,-2.82284719206225,302.244874074203));
#7832=CARTESIAN_POINT('Ctrl Pts',(2.65654986806645,-2.90253669097776,302.239005843219));
#7833=CARTESIAN_POINT('Ctrl Pts',(2.56860277056448,-2.97838358964195,302.233137612236));
#7834=CARTESIAN_POINT('Ctrl Pts',(2.47896516745839,-3.05568840574616,302.227156583017));
#7835=CARTESIAN_POINT('Ctrl Pts',(2.38576741288148,-3.12900103385408,302.221175553799));
#7836=CARTESIAN_POINT('Ctrl Pts',(2.28940502272061,-3.19798587269263,302.215194524581));
#7837=CARTESIAN_POINT('Ctrl Pts',(2.19496397897108,-3.26559523949984,302.209332749658));
#7838=CARTESIAN_POINT('Ctrl Pts',(2.0974836784843,-3.32904754989813,302.203470974736));
#7839=CARTESIAN_POINT('Ctrl Pts',(1.99736905234799,-3.38806816175863,302.197609199814));
#7840=CARTESIAN_POINT('Ctrl Pts',(1.8972682719864,-3.44708061111453,302.191748235571));
#7841=CARTESIAN_POINT('Ctrl Pts',(1.79453424516496,-3.50166237172745,302.185887271328));
#7842=CARTESIAN_POINT('Ctrl Pts',(1.68959894593192,-3.55158336547317,302.180026307084));
#7843=CARTESIAN_POINT('Ctrl Pts',(1.58465298500415,-3.60150943131951,302.174164747352));
#7844=CARTESIAN_POINT('Ctrl Pts',(1.47750567892787,-3.64677361201655,302.16830318762));
#7845=CARTESIAN_POINT('Ctrl Pts',(1.3686109082234,-3.68719313053872,302.162441627888));
#7846=CARTESIAN_POINT('Ctrl Pts',(1.25583028490952,-3.729054998317,302.15637090148));
#7847=CARTESIAN_POINT('Ctrl Pts',(1.141175598582,-3.76571981855618,302.150300175072));
#7848=CARTESIAN_POINT('Ctrl Pts',(1.02516910154346,-3.7970405993669,302.144229448664));
#7849=CARTESIAN_POINT('Ctrl Pts',(0.912994508079632,-3.82732679836527,302.138359249286));
#7850=CARTESIAN_POINT('Ctrl Pts',(0.799556420830987,-3.85261639866862,302.132489049907));
#7851=CARTESIAN_POINT('Ctrl Pts',(0.685337119420493,-3.87282868621172,302.126618850529));
#7852=CARTESIAN_POINT('Ctrl Pts',(0.565265191280603,-3.8940766566287,302.120447860606));
#7853=CARTESIAN_POINT('Ctrl Pts',(0.44433039437697,-3.90971313830006,302.114276870684));
#7854=CARTESIAN_POINT('Ctrl Pts',(0.32309730988824,-3.91970625536442,302.108105880761));
#7855=CARTESIAN_POINT('Ctrl Pts',(0.20186422539951,-3.92969937242878,302.101934890839));
#7856=CARTESIAN_POINT('Ctrl Pts',(0.0803333767019532,-3.93404917677253,
302.095763900916));
#7857=CARTESIAN_POINT('Ctrl Pts',(-0.0409340283512824,-3.93278697685534,
302.089592910994));
#7858=CARTESIAN_POINT('Ctrl Pts',(-0.156513224452078,-3.93158398210432,
302.083711379563));
#7859=CARTESIAN_POINT('Ctrl Pts',(-0.272225530854058,-3.92527967244628,
302.077829848132));
#7860=CARTESIAN_POINT('Ctrl Pts',(-0.387584714775374,-3.9138557828403,302.071948316701));
#7861=CARTESIAN_POINT('Ctrl Pts',(-0.50279810788512,-3.90244633073363,302.066074218343));
#7862=CARTESIAN_POINT('Ctrl Pts',(-0.617658859820622,-3.88593020698841,
302.060200119985));
#7863=CARTESIAN_POINT('Ctrl Pts',(-0.731680582857664,-3.86434115014048,
302.054326021627));
#7864=CARTESIAN_POINT('Ctrl Pts',(-0.845588414685746,-3.84277365763765,
302.048457790644));
#7865=CARTESIAN_POINT('Ctrl Pts',(-0.958658482396879,-3.81614338804557,
302.04258955966));
#7866=CARTESIAN_POINT('Ctrl Pts',(-1.07041001841095,-3.78453582259244,302.036721328677));
#7867=CARTESIAN_POINT('Ctrl Pts',(-1.18430962529428,-3.75232070136855,302.030740299458));
#7868=CARTESIAN_POINT('Ctrl Pts',(-1.29683905491205,-3.71493500399161,302.02475927024));
#7869=CARTESIAN_POINT('Ctrl Pts',(-1.40750032594185,-3.67252390495604,302.018778241021));
#7870=CARTESIAN_POINT('Ctrl Pts',(-1.51595514862634,-3.63095843057686,302.0129164661));
#7871=CARTESIAN_POINT('Ctrl Pts',(-1.62261521870106,-3.58456625312323,302.007054691177));
#7872=CARTESIAN_POINT('Ctrl Pts',(-1.72702824034959,-3.53353398979478,302.001192916255));
#7873=CARTESIAN_POINT('Ctrl Pts',(-1.83142682175857,-3.48250878418858,301.995331952012));
#7874=CARTESIAN_POINT('Ctrl Pts',(-1.93357860287678,-3.42684494967867,301.989470987769));
#7875=CARTESIAN_POINT('Ctrl Pts',(-2.03305357901847,-3.36677622434878,301.983610023526));
#7876=CARTESIAN_POINT('Ctrl Pts',(-2.13253866207163,-3.30670139588306,301.977748463794));
#7877=CARTESIAN_POINT('Ctrl Pts',(-2.22934604697232,-3.24222099977972,301.971886904062));
#7878=CARTESIAN_POINT('Ctrl Pts',(-2.32307313431842,-3.17361311640345,301.96602534433));
#7879=CARTESIAN_POINT('Ctrl Pts',(-2.42014482347843,-3.10255699679487,301.959954617922));
#7880=CARTESIAN_POINT('Ctrl Pts',(-2.51391188486858,-3.02707359239639,301.953883891514));
#7881=CARTESIAN_POINT('Ctrl Pts',(-2.60396391385376,-2.94751775827516,301.947813165106));
#7882=CARTESIAN_POINT('Ctrl Pts',(-2.69104136209353,-2.87058979667417,301.941942965728));
#7883=CARTESIAN_POINT('Ctrl Pts',(-2.7746450727689,-2.78985453125091,301.936072766349));
#7884=CARTESIAN_POINT('Ctrl Pts',(-2.85444197557788,-2.705669973973,301.930202566971));
#7885=CARTESIAN_POINT('Ctrl Pts',(-2.93832769246163,-2.61717177806302,301.924031577048));
#7886=CARTESIAN_POINT('Ctrl Pts',(-3.01800579814773,-2.52486184285643,301.917860587125));
#7887=CARTESIAN_POINT('Ctrl Pts',(-3.09313863580993,-2.42919377153407,301.911689597202));
#7888=CARTESIAN_POINT('Ctrl Pts',(-3.16827147347212,-2.3335257002117,301.90551860728));
#7889=CARTESIAN_POINT('Ctrl Pts',(-3.23885879805824,-2.23449995813832,301.899347617357));
#7890=CARTESIAN_POINT('Ctrl Pts',(-3.30461754106511,-2.13260214463101,301.893176627434));
#7891=CARTESIAN_POINT('Ctrl Pts',(-3.36729178276125,-2.03548398360718,301.887295096002));
#7892=CARTESIAN_POINT('Ctrl Pts',(-3.42578211398755,-1.93544417487477,301.88141356457));
#7893=CARTESIAN_POINT('Ctrl Pts',(-3.47980540261538,-1.83287843566583,301.875532033138));
#7894=CARTESIAN_POINT('Ctrl Pts',(-3.53376041666969,-1.73044231892676,301.869657934779));
#7895=CARTESIAN_POINT('Ctrl Pts',(-3.58325942579112,-1.62548698185613,301.86378383642));
#7896=CARTESIAN_POINT('Ctrl Pts',(-3.62806261151043,-1.51843692228557,301.857909738061));
#7897=CARTESIAN_POINT('Ctrl Pts',(-3.67282104532781,-1.41149379024019,301.852041507076));
#7898=CARTESIAN_POINT('Ctrl Pts',(-3.71289282816416,-1.30246047562573,301.846173276092));
#7899=CARTESIAN_POINT('Ctrl Pts',(-3.74808441926684,-1.19178529360331,301.840305045107));
#7900=CARTESIAN_POINT('Ctrl Pts',(-3.78395245772235,-1.07898273025041,301.834324015889));
#7901=CARTESIAN_POINT('Ctrl Pts',(-3.81475055041141,-0.964474912250716,
301.828342986671));
#7902=CARTESIAN_POINT('Ctrl Pts',(-3.84032548906766,-0.848757408225265,
301.822361957453));
#7903=CARTESIAN_POINT('Ctrl Pts',(-3.86539049520763,-0.735347167524981,
301.81650018253));
#7904=CARTESIAN_POINT('Ctrl Pts',(-3.88543861199051,-0.620775453322663,
301.810638407607));
#7905=CARTESIAN_POINT('Ctrl Pts',(-3.90037638707522,-0.505522540690357,
301.804776632684));
#7906=CARTESIAN_POINT('Ctrl Pts',(-3.91531209627727,-0.390285567446099,
301.79891566844));
#7907=CARTESIAN_POINT('Ctrl Pts',(-3.92513881639053,-0.274367991409209,
301.793054704196));
#7908=CARTESIAN_POINT('Ctrl Pts',(-3.92981470056569,-0.158257446010553,
301.787193739952));
#7909=CARTESIAN_POINT('Ctrl Pts',(-3.93449105982262,-0.0421351034841711,
301.781332180218));
#7910=CARTESIAN_POINT('Ctrl Pts',(-3.93401552621659,0.0741798359052884,
301.775470620485));
#7911=CARTESIAN_POINT('Ctrl Pts',(-3.92839835717182,0.190198179196717,301.769609060752));
#7912=CARTESIAN_POINT('Ctrl Pts',(-3.92258074240665,0.310356575994506,301.763538334346));
#7913=CARTESIAN_POINT('Ctrl Pts',(-3.91124770501772,0.430196337331117,301.757467607939));
#7914=CARTESIAN_POINT('Ctrl Pts',(-3.89446927364822,0.54917945756368,301.751396881533));
#7915=CARTESIAN_POINT('Ctrl Pts',(-3.87824506408611,0.664232351037048,301.745526682153));
#7916=CARTESIAN_POINT('Ctrl Pts',(-3.85692965953988,0.778483902690411,301.739656482774));
#7917=CARTESIAN_POINT('Ctrl Pts',(-3.83063833044708,0.891458906125011,301.733786283394));
#7918=CARTESIAN_POINT('Ctrl Pts',(-3.80299982682417,1.01022277807323,301.727615293474));
#7919=CARTESIAN_POINT('Ctrl Pts',(-3.76986210004843,1.12757530558744,301.721444303554));
#7920=CARTESIAN_POINT('Ctrl Pts',(-3.73141766823532,1.24298478879724,301.715273313634));
#7921=CARTESIAN_POINT('Ctrl Pts',(-3.6929732364222,1.35839427200703,301.709102323714));
#7922=CARTESIAN_POINT('Ctrl Pts',(-3.64922235292573,1.47186025001474,301.702931333794));
#7923=CARTESIAN_POINT('Ctrl Pts',(-3.60041431324824,1.58287895082258,301.696760343874));
#7924=CARTESIAN_POINT('Ctrl Pts',(-3.55389567958219,1.68869017182402,301.690878812443));
#7925=CARTESIAN_POINT('Ctrl Pts',(-3.5026336969854,1.79261943292805,301.684997281012));
#7926=CARTESIAN_POINT('Ctrl Pts',(-3.44680261578062,1.89421242944076,301.679115749581));
#7927=CARTESIAN_POINT('Ctrl Pts',(-3.39104209383567,1.99567703283474,301.673241651223));
#7928=CARTESIAN_POINT('Ctrl Pts',(-3.33072415434749,2.0948108860578,301.667367552865));
#7929=CARTESIAN_POINT('Ctrl Pts',(-3.26607092977496,2.19117997473482,301.661493454507));
#7930=CARTESIAN_POINT('Ctrl Pts',(-3.20148228442217,2.28745280463135,301.655625223524));
#7931=CARTESIAN_POINT('Ctrl Pts',(-3.13256719626732,2.38096602345882,301.649756992541));
#7932=CARTESIAN_POINT('Ctrl Pts',(-3.05959317090488,2.47131111528926,301.643888761557));
#7933=CARTESIAN_POINT('Ctrl Pts',(-2.98521645002921,2.56339280660591,301.637907732339));
#7934=CARTESIAN_POINT('Ctrl Pts',(-2.90662334810153,2.65218293684628,301.63192670312));
#7935=CARTESIAN_POINT('Ctrl Pts',(-2.82414302670634,2.73728061489975,301.625945673902));
#7936=CARTESIAN_POINT('Ctrl Pts',(-2.743307260511,2.82068155091134,301.62008389898));
#7937=CARTESIAN_POINT('Ctrl Pts',(-2.65873815131181,2.9005356080816,301.614222124058));
#7938=CARTESIAN_POINT('Ctrl Pts',(-2.57078502006558,2.97650018992212,301.608360349136));
#7939=CARTESIAN_POINT('Ctrl Pts',(-2.48284405266893,3.05245426592011,301.602499384893));
#7940=CARTESIAN_POINT('Ctrl Pts',(-2.39152030552613,3.12451966722843,301.59663842065));
#7941=CARTESIAN_POINT('Ctrl Pts',(-2.29719767240283,3.19239281008885,301.590777456407));
#7942=CARTESIAN_POINT('Ctrl Pts',(-2.202865455859,3.26027284903402,301.584915896675));
#7943=CARTESIAN_POINT('Ctrl Pts',(-2.10553408188822,3.32395954225842,301.579054336943));
#7944=CARTESIAN_POINT('Ctrl Pts',(-2.0056174525181,3.383191929843,301.573192777211));
#7945=CARTESIAN_POINT('Ctrl Pts',(-1.90213535078211,3.44453799402405,301.567122050803));
#7946=CARTESIAN_POINT('Ctrl Pts',(-1.79588044885803,3.50110566993863,301.561051324394));
#7947=CARTESIAN_POINT('Ctrl Pts',(-1.68734031573684,3.55265698581908,301.554980597986));
#7948=CARTESIAN_POINT('Ctrl Pts',(-1.58238545874679,3.60250546886673,301.549110398608));
#7949=CARTESIAN_POINT('Ctrl Pts',(-1.47529436655568,3.64766365189979,301.54324019923));
#7950=CARTESIAN_POINT('Ctrl Pts',(-1.36652712562136,3.68796591835405,301.537369999851));
#7951=CARTESIAN_POINT('Ctrl Pts',(-1.2521866229445,3.73033328343394,301.531199009928));
#7952=CARTESIAN_POINT('Ctrl Pts',(-1.1359941536543,3.76733375293836,301.525028020005));
#7953=CARTESIAN_POINT('Ctrl Pts',(-1.01849950972214,3.79883505152511,301.518857030082));
#7954=CARTESIAN_POINT('Ctrl Pts',(-0.901004865789978,3.83033635011185,301.51268604016));
#7955=CARTESIAN_POINT('Ctrl Pts',(-0.782208571438065,3.85633843528389,301.506515050237));
#7956=CARTESIAN_POINT('Ctrl Pts',(-0.662668393150373,3.876771801476,301.500344060314));
#7957=CARTESIAN_POINT('Ctrl Pts',(-0.548735405950678,3.89624671344418,301.494462528883));
#7958=CARTESIAN_POINT('Ctrl Pts',(-0.433759646993851,3.91072625163271,301.488580997451));
#7959=CARTESIAN_POINT('Ctrl Pts',(-0.318216254326227,3.92010553626845,301.48269946602));
#7960=CARTESIAN_POINT('Ctrl Pts',(-0.202818885273205,3.92947296737443,301.476825367662));
#7961=CARTESIAN_POINT('Ctrl Pts',(-0.0868557161747232,3.93375293139621,
301.470951269304));
#7962=CARTESIAN_POINT('Ctrl Pts',(0.0291886673973893,3.93289168700278,301.465077170946));
#7963=CARTESIAN_POINT('Ctrl Pts',(0.145117139415245,3.93203130286792,301.459208939962));
#7964=CARTESIAN_POINT('Ctrl Pts',(0.261126255042988,3.92603992884983,301.453340708978));
#7965=CARTESIAN_POINT('Ctrl Pts',(0.376727709900824,3.91491573761082,301.447472477995));
#7966=CARTESIAN_POINT('Ctrl Pts',(0.494551238172704,3.90357771887599,301.441491448777));
#7967=CARTESIAN_POINT('Ctrl Pts',(0.61195083854817,3.8869074840324,301.435510419558));
#7968=CARTESIAN_POINT('Ctrl Pts',(0.728410600579671,3.86495886096646,301.42952939034));
#7969=CARTESIAN_POINT('Ctrl Pts',(0.842548299559075,3.84344786619184,301.423667615417));
#7970=CARTESIAN_POINT('Ctrl Pts',(0.955782868850346,3.81686710255977,301.417805840495));
#7971=CARTESIAN_POINT('Ctrl Pts',(1.06763594037823,3.78531933907995,301.411944065573));
#7972=CARTESIAN_POINT('Ctrl Pts',(1.17947354271343,3.75377593863126,301.40608310133));
#7973=CARTESIAN_POINT('Ctrl Pts',(1.28992963100695,3.7172670161951,301.400222137087));
#7974=CARTESIAN_POINT('Ctrl Pts',(1.39853934699904,3.67594568715256,301.394361172843));
#7975=CARTESIAN_POINT('Ctrl Pts',(1.50716009801596,3.63462015975734,301.388499613111));
#7976=CARTESIAN_POINT('Ctrl Pts',(1.61393371891261,3.58848140019164,301.382638053379));
#7977=CARTESIAN_POINT('Ctrl Pts',(1.71841438968721,3.5377310504497,301.376776493647));
#7978=CARTESIAN_POINT('Ctrl Pts',(1.82662339823676,3.48516970117424,301.370705767239));
#7979=CARTESIAN_POINT('Ctrl Pts',(1.93237232452568,3.42766169539426,301.364635040831));
#7980=CARTESIAN_POINT('Ctrl Pts',(2.03519394636125,3.3654828183627,301.358564314423));
#7981=CARTESIAN_POINT('Ctrl Pts',(2.13461918480164,3.30535782165038,301.352694115045));
#7982=CARTESIAN_POINT('Ctrl Pts',(2.23130713953981,3.24086593897699,301.346823915666));
#7983=CARTESIAN_POINT('Ctrl Pts',(2.32486611309963,3.17229988433645,301.340953716287));
#7984=CARTESIAN_POINT('Ctrl Pts',(2.42321907281305,3.10022048721204,301.334782726365));
#7985=CARTESIAN_POINT('Ctrl Pts',(2.51811348592935,3.0236386680859,301.328611736443));
#7986=CARTESIAN_POINT('Ctrl Pts',(2.60913605640942,2.94294037301885,301.32244074652));
#7987=CARTESIAN_POINT('Ctrl Pts',(2.70015862688948,2.8622420779518,301.316269756598));
#7988=CARTESIAN_POINT('Ctrl Pts',(2.78730903044843,2.77742772101416,301.310098766675));
#7989=CARTESIAN_POINT('Ctrl Pts',(2.87022196134222,2.68892448622657,301.303927776753));
#7990=CARTESIAN_POINT('Ctrl Pts',(2.94828653660491,2.6055965015734,301.298117637103));
#7991=CARTESIAN_POINT('Ctrl Pts',(3.02286069147831,2.51871501896711,301.292307497454));
#7992=CARTESIAN_POINT('Ctrl Pts',(3.09359853530955,2.42860805860695,301.286497357804));
#7993=CARTESIAN_POINT('Ctrl Pts',(3.16422565332073,2.3386421425102,301.280696312756));
#7994=CARTESIAN_POINT('Ctrl Pts',(3.23102815063106,2.24546112486799,301.274895267708));
#7995=CARTESIAN_POINT('Ctrl Pts',(3.29369747789793,2.14942920890379,301.269094222659));
#7996=CARTESIAN_POINT('Ctrl Pts',(3.3563107355319,2.05348321175363,301.263298367749));
#7997=CARTESIAN_POINT('Ctrl Pts',(3.41479794135421,1.95469173649733,301.257502512839));
#7998=CARTESIAN_POINT('Ctrl Pts',(3.46889144557637,1.85345114281631,301.251706657929));
#7999=CARTESIAN_POINT('Ctrl Pts',(3.52295033287159,1.75227533765814,301.245914512053));
#8000=CARTESIAN_POINT('Ctrl Pts',(3.57262090867942,1.64865390115011,301.240122366178));
#8001=CARTESIAN_POINT('Ctrl Pts',(3.6176798727907,1.54301047890321,301.234330220302));
#8002=CARTESIAN_POINT('Ctrl Pts',(3.66272147733844,1.43740775718586,301.228540305928));
#8003=CARTESIAN_POINT('Ctrl Pts',(3.70315483784618,1.32978498747829,301.222750391554));
#8004=CARTESIAN_POINT('Ctrl Pts',(3.73880385742427,1.22058785661229,301.216960477179));
#8005=CARTESIAN_POINT('Ctrl Pts',(3.77445892735166,1.11137219281629,301.211169580141));
#8006=CARTESIAN_POINT('Ctrl Pts',(3.80532789413077,1.00058203347094,301.205378683103));
#8007=CARTESIAN_POINT('Ctrl Pts',(3.83128397436347,0.888679980524858,301.199587786064));
#8008=CARTESIAN_POINT('Ctrl Pts',(3.85724201819696,0.776769462087923,301.193796450939));
#8009=CARTESIAN_POINT('Ctrl Pts',(3.87828634872675,0.663747296822126,301.188005115815));
#8010=CARTESIAN_POINT('Ctrl Pts',(3.89434122249579,0.550086759311637,301.18221378069));
#8011=CARTESIAN_POINT('Ctrl Pts',(3.9104088514833,0.436335921185449,301.176417844486));
#8012=CARTESIAN_POINT('Ctrl Pts',(3.92147905828884,0.32194611844812,301.170621908282));
#8013=CARTESIAN_POINT('Ctrl Pts',(3.92752796032574,0.207396048321935,301.164825972078));
#8014=CARTESIAN_POINT('Ctrl Pts',(3.93123723255074,0.137152326254839,301.161271822077));
#8015=CARTESIAN_POINT('Ctrl Pts',(3.93305935886409,0.0668483962409372,301.157717672076));
#8016=CARTESIAN_POINT('Ctrl Pts',(3.93299852553402,-0.00340560526561647,
301.154163522075));
#8017=CARTESIAN_POINT('',(3.93299918092051,0.00253828261005724,299.904163521993));
#8018=CARTESIAN_POINT('Ctrl Pts',(3.93299852553333,-0.00340560606263315,
301.154163522035));
#8019=CARTESIAN_POINT('Ctrl Pts',(3.93286544172368,-0.157098786510854,301.146388183894));
#8020=CARTESIAN_POINT('Ctrl Pts',(3.92371953772783,-0.310406465359547,301.138612845754));
#8021=CARTESIAN_POINT('Ctrl Pts',(3.9057186758342,-0.462439861214385,301.130837507614));
#8022=CARTESIAN_POINT('Ctrl Pts',(3.88771781394057,-0.614473257069218,301.123062169474));
#8023=CARTESIAN_POINT('Ctrl Pts',(3.86086214198175,-0.76523283790746,301.115286831334));
#8024=CARTESIAN_POINT('Ctrl Pts',(3.82535752409155,-0.913853824676678,301.107511493194));
#8025=CARTESIAN_POINT('Ctrl Pts',(3.79850061804613,-1.0262758169477,301.101629961768));
#8026=CARTESIAN_POINT('Ctrl Pts',(3.76664036763773,-1.13769397793598,301.095748430341));
#8027=CARTESIAN_POINT('Ctrl Pts',(3.7298670150837,-1.24763017348516,301.089866898915));
#8028=CARTESIAN_POINT('Ctrl Pts',(3.69314013665271,-1.35742743178973,301.083992800562));
#8029=CARTESIAN_POINT('Ctrl Pts',(3.65151263467781,-1.46574606240973,301.078118702208));
#8030=CARTESIAN_POINT('Ctrl Pts',(3.60512548911743,-1.5721193363469,301.072244603855));
#8031=CARTESIAN_POINT('Ctrl Pts',(3.55878467760578,-1.67838635876979,301.066376372876));
#8032=CARTESIAN_POINT('Ctrl Pts',(3.50769384352751,-1.78271151453515,301.060508141897));
#8033=CARTESIAN_POINT('Ctrl Pts',(3.45204316688197,-1.88464505251878,301.054639910918));
#8034=CARTESIAN_POINT('Ctrl Pts',(3.39532278141295,-1.9885379414315,301.048658881698));
#8035=CARTESIAN_POINT('Ctrl Pts',(3.33386558241176,-2.08994590758908,301.042677852478));
#8036=CARTESIAN_POINT('Ctrl Pts',(3.26792377584436,-2.18841568155392,301.036696823258));
#8037=CARTESIAN_POINT('Ctrl Pts',(3.20329676709334,-2.28492209038627,301.03083504834));
#8038=CARTESIAN_POINT('Ctrl Pts',(3.134362568962,-2.37860603237732,301.024973273423));
#8039=CARTESIAN_POINT('Ctrl Pts',(3.0614036416859,-2.46906799069453,301.019111498505));
#8040=CARTESIAN_POINT('Ctrl Pts',(2.98845480457217,-2.5595174381939,301.013250534266));
#8041=CARTESIAN_POINT('Ctrl Pts',(2.91148260371487,-2.64674546771846,301.007389570028));
#8042=CARTESIAN_POINT('Ctrl Pts',(2.83081048851926,-2.73038476740721,301.001528605789));
#8043=CARTESIAN_POINT('Ctrl Pts',(2.75013017683002,-2.81403256506314,300.995667046061));
#8044=CARTESIAN_POINT('Ctrl Pts',(2.66574948938891,-2.89409061163738,300.989805486334));
#8045=CARTESIAN_POINT('Ctrl Pts',(2.57802901917603,-2.97022816906147,300.983943926606));
#8046=CARTESIAN_POINT('Ctrl Pts',(2.48717828995953,-3.04908265531714,300.977873200191));
#8047=CARTESIAN_POINT('Ctrl Pts',(2.3927453270273,-3.12373131025809,300.971802473777));
#8048=CARTESIAN_POINT('Ctrl Pts',(2.29516731291217,-3.19385284660072,300.965731747362));
#8049=CARTESIAN_POINT('Ctrl Pts',(2.20081247655601,-3.26165814215475,300.959861547988));
#8050=CARTESIAN_POINT('Ctrl Pts',(2.10351746537517,-3.32523049700673,300.953991348614));
#8051=CARTESIAN_POINT('Ctrl Pts',(2.00370535464434,-3.38432472611149,300.94812114924));
#8052=CARTESIAN_POINT('Ctrl Pts',(1.89877884510035,-3.44644695906252,300.941950159305));
#8053=CARTESIAN_POINT('Ctrl Pts',(1.79107091742521,-3.50361974134937,300.935779169371));
#8054=CARTESIAN_POINT('Ctrl Pts',(1.68109886722079,-3.55561465834376,300.929608179436));
#8055=CARTESIAN_POINT('Ctrl Pts',(1.57112681701637,-3.60760957533814,300.923437189501));
#8056=CARTESIAN_POINT('Ctrl Pts',(1.45889115246718,-3.65442649152832,300.917266199567));
#8057=CARTESIAN_POINT('Ctrl Pts',(1.34492823469044,-3.69589732589157,300.911095209632));
#8058=CARTESIAN_POINT('Ctrl Pts',(1.23631089938217,-3.73542291552566,300.905213678201));
#8059=CARTESIAN_POINT('Ctrl Pts',(1.12577471544002,-3.77021995865531,300.89933214677));
#8060=CARTESIAN_POINT('Ctrl Pts',(1.01376842338997,-3.80010033864073,300.893450615339));
#8061=CARTESIAN_POINT('Ctrl Pts',(0.90190368477125,-3.8299429558341,300.887576516981));
#8062=CARTESIAN_POINT('Ctrl Pts',(0.788572927624833,-3.85488116269691,300.881702418622));
#8063=CARTESIAN_POINT('Ctrl Pts',(0.674243328308639,-3.87477546887962,300.875828320264));
#8064=CARTESIAN_POINT('Ctrl Pts',(0.560027927726205,-3.89464990352785,300.869960089281));
#8065=CARTESIAN_POINT('Ctrl Pts',(0.444816073097176,-3.90949038943803,300.864091858297));
#8066=CARTESIAN_POINT('Ctrl Pts',(0.329087878767785,-3.91920784955941,300.858223627314));
#8067=CARTESIAN_POINT('Ctrl Pts',(0.211135174855668,-3.92911209720724,300.852242598096));
#8068=CARTESIAN_POINT('Ctrl Pts',(0.092646496011925,-3.93369422362777,300.846261568877));
#8069=CARTESIAN_POINT('Ctrl Pts',(-0.0258609341332851,-3.93291497646285,
300.840280539659));
#8070=CARTESIAN_POINT('Ctrl Pts',(-0.142005473262481,-3.93215126651886,
300.834418764737));
#8071=CARTESIAN_POINT('Ctrl Pts',(-0.258167592749956,-3.92623800412594,
300.828556989815));
#8072=CARTESIAN_POINT('Ctrl Pts',(-0.373858259075998,-3.91519080021915,
300.822695214893));
#8073=CARTESIAN_POINT('Ctrl Pts',(-0.48953292547211,-3.90414512413214,300.81683425065));
#8074=CARTESIAN_POINT('Ctrl Pts',(-0.604735858539051,-3.88796695768332,
300.810973286407));
#8075=CARTESIAN_POINT('Ctrl Pts',(-0.718982318146374,-3.86672386215939,
300.805112322164));
#8076=CARTESIAN_POINT('Ctrl Pts',(-0.833240385484909,-3.84547860828287,
300.799250762432));
#8077=CARTESIAN_POINT('Ctrl Pts',(-0.946541381309225,-3.81916747760979,
300.793389202701));
#8078=CARTESIAN_POINT('Ctrl Pts',(-1.05841062355543,-3.78790917947421,300.787527642969));
#8079=CARTESIAN_POINT('Ctrl Pts',(-1.17427186087287,-3.75553544541017,300.781456916561));
#8080=CARTESIAN_POINT('Ctrl Pts',(-1.28859679337923,-3.71785500023334,300.775386190153));
#8081=CARTESIAN_POINT('Ctrl Pts',(-1.40087642916247,-3.67505567715878,300.769315463745));
#8082=CARTESIAN_POINT('Ctrl Pts',(-1.5094472663012,-3.63367009282944,300.763445264367));
#8083=CARTESIAN_POINT('Ctrl Pts',(-1.61610543337552,-3.58749868482146,300.757575064989));
#8084=CARTESIAN_POINT('Ctrl Pts',(-1.72041322114692,-3.53675944170689,300.751704865611));
#8085=CARTESIAN_POINT('Ctrl Pts',(-1.83006576712542,-3.48342030656267,300.745533875688));
#8086=CARTESIAN_POINT('Ctrl Pts',(-1.93712022061616,-3.42503307634353,300.739362885765));
#8087=CARTESIAN_POINT('Ctrl Pts',(-2.04110095740411,-3.36190360981454,300.733191895842));
#8088=CARTESIAN_POINT('Ctrl Pts',(-2.14508169419205,-3.29877414328555,300.727020905919));
#8089=CARTESIAN_POINT('Ctrl Pts',(-2.24598832120386,-3.23090278988663,300.720849915996));
#8090=CARTESIAN_POINT('Ctrl Pts',(-2.3433850608668,-3.15864456001404,300.714678926073));
#8091=CARTESIAN_POINT('Ctrl Pts',(-2.43621327726425,-3.08977569826034,300.708797394618));
#8092=CARTESIAN_POINT('Ctrl Pts',(-2.52615252292027,-3.01670029628729,300.702915863163));
#8093=CARTESIAN_POINT('Ctrl Pts',(-2.61279857418619,-2.93968920308434,300.697034331708));
#8094=CARTESIAN_POINT('Ctrl Pts',(-2.6993351222681,-2.86277543641601,300.691160233326));
#8095=CARTESIAN_POINT('Ctrl Pts',(-2.78258644826526,-2.78193614210238,300.685286134944));
#8096=CARTESIAN_POINT('Ctrl Pts',(-2.86217875188137,-2.69748434514064,300.679412036562));
#8097=CARTESIAN_POINT('Ctrl Pts',(-2.9416915542995,-2.61311690330777,300.673543805554));
#8098=CARTESIAN_POINT('Ctrl Pts',(-3.01755232388958,-2.52514443481699,300.667675574547));
#8099=CARTESIAN_POINT('Ctrl Pts',(-3.08942220406522,-2.43391853705682,300.661807343539));
#8100=CARTESIAN_POINT('Ctrl Pts',(-3.16267355563161,-2.34093910961853,300.65582631433));
#8101=CARTESIAN_POINT('Ctrl Pts',(-3.23177868287738,-2.24458017523864,300.64984528512));
#8102=CARTESIAN_POINT('Ctrl Pts',(-3.29641986457654,-2.14525175129288,300.643864255911));
#8103=CARTESIAN_POINT('Ctrl Pts',(-3.35977218172926,-2.0479038122441,300.638002480965));
#8104=CARTESIAN_POINT('Ctrl Pts',(-3.41883668120434,-1.94770406333801,300.632140706019));
#8105=CARTESIAN_POINT('Ctrl Pts',(-3.47335695864057,-1.84506922305455,300.626278931072));
#8106=CARTESIAN_POINT('Ctrl Pts',(-3.52786969596439,-1.74244857709051,300.620417966805));
#8107=CARTESIAN_POINT('Ctrl Pts',(-3.57783926793467,-1.63739387307015,300.614557002538));
#8108=CARTESIAN_POINT('Ctrl Pts',(-3.62305499023294,-1.53034686844134,300.608696038271));
#8109=CARTESIAN_POINT('Ctrl Pts',(-3.66827530656344,-1.42328898756495,300.602834478515));
#8110=CARTESIAN_POINT('Ctrl Pts',(-3.70874065281395,-1.3142387830344,300.596972918758));
#8111=CARTESIAN_POINT('Ctrl Pts',(-3.74428857119481,-1.20365779838788,300.591111359002));
#8112=CARTESIAN_POINT('Ctrl Pts',(-3.78110499798921,-1.08913079057624,300.585040632628));
#8113=CARTESIAN_POINT('Ctrl Pts',(-3.8126463413861,-0.972962164740077,300.578969906254));
#8114=CARTESIAN_POINT('Ctrl Pts',(-3.8387889272288,-0.85568018101715,300.57289917988));
#8115=CARTESIAN_POINT('Ctrl Pts',(-3.86406797660831,-0.74227223140965,300.567028980478));
#8116=CARTESIAN_POINT('Ctrl Pts',(-3.88429928560468,-0.627823737477159,
300.561158781076));
#8117=CARTESIAN_POINT('Ctrl Pts',(-3.89942361896982,-0.512820085234843,
300.555288581674));
#8118=CARTESIAN_POINT('Ctrl Pts',(-3.91532292688877,-0.391923617624727,
300.549117591814));
#8119=CARTESIAN_POINT('Ctrl Pts',(-3.92557798633627,-0.270414119568538,
300.542946601953));
#8120=CARTESIAN_POINT('Ctrl Pts',(-3.93018200398618,-0.148857030546762,
300.536775612093));
#8121=CARTESIAN_POINT('Ctrl Pts',(-3.93478602163608,-0.0272999415249911,
300.530604622233));
#8122=CARTESIAN_POINT('Ctrl Pts',(-3.9337390725465,0.0943042179038661,300.524433632373));
#8123=CARTESIAN_POINT('Ctrl Pts',(-3.92709733580095,0.215396181825655,300.518262642513));
#8124=CARTESIAN_POINT('Ctrl Pts',(-3.92076713854647,0.330808166209259,300.512381111135));
#8125=CARTESIAN_POINT('Ctrl Pts',(-3.90933474442532,0.446126778362399,300.506499579757));
#8126=CARTESIAN_POINT('Ctrl Pts',(-3.89280348111259,0.560865453952848,300.50061804838));
#8127=CARTESIAN_POINT('Ctrl Pts',(-3.87629310999253,0.67545912292934,300.494743950075));
#8128=CARTESIAN_POINT('Ctrl Pts',(-3.85469674392071,0.789473908932605,300.488869851771));
#8129=CARTESIAN_POINT('Ctrl Pts',(-3.82806966980634,0.902425400301178,300.482995753466));
#8130=CARTESIAN_POINT('Ctrl Pts',(-3.80146919228729,1.0152640694688,300.477127522536));
#8131=CARTESIAN_POINT('Ctrl Pts',(-3.76984809661646,1.12704115817196,300.471259291606));
#8132=CARTESIAN_POINT('Ctrl Pts',(-3.7333131120623,1.23728016524299,300.465391060676));
#8133=CARTESIAN_POINT('Ctrl Pts',(-3.69607585718077,1.3496381709814,300.459410031437));
#8134=CARTESIAN_POINT('Ctrl Pts',(-3.65373391493465,1.46039792426789,300.453429002199));
#8135=CARTESIAN_POINT('Ctrl Pts',(-3.60645441286819,1.56906837578977,300.44744797296));
#8136=CARTESIAN_POINT('Ctrl Pts',(-3.56011760594133,1.67557207212198,300.441586198091));
#8137=CARTESIAN_POINT('Ctrl Pts',(-3.50903848509052,1.78006861691531,300.435724423222));
#8138=CARTESIAN_POINT('Ctrl Pts',(-3.45342355262258,1.88211444024842,300.429862648352));
#8139=CARTESIAN_POINT('Ctrl Pts',(-3.39781631165343,1.98414615072926,300.424001684162));
#8140=CARTESIAN_POINT('Ctrl Pts',(-3.33767470359273,2.08372745228817,300.418140719971));
#8141=CARTESIAN_POINT('Ctrl Pts',(-3.27325131613854,2.18043913499032,300.41227975578));
#8142=CARTESIAN_POINT('Ctrl Pts',(-3.20882138309925,2.27716064385303,300.4064181961));
#8143=CARTESIAN_POINT('Ctrl Pts',(-3.14010903414613,2.37101161153109,300.40055663642));
#8144=CARTESIAN_POINT('Ctrl Pts',(-3.06740993958069,2.46160217390251,300.39469507674));
#8145=CARTESIAN_POINT('Ctrl Pts',(-2.99211661447514,2.55542541482317,300.388624350257));
#8146=CARTESIAN_POINT('Ctrl Pts',(-2.91254699513114,2.64575083864331,300.382553623775));
#8147=CARTESIAN_POINT('Ctrl Pts',(-2.82907379728921,2.73218419025724,300.376482897293));
#8148=CARTESIAN_POINT('Ctrl Pts',(-2.74835787123007,2.81576249081697,300.370612697965));
#8149=CARTESIAN_POINT('Ctrl Pts',(-2.66399252507181,2.8957015404752,300.364742498637));
#8150=CARTESIAN_POINT('Ctrl Pts',(-2.57635019690619,2.97168448239403,300.358872299309));
#8151=CARTESIAN_POINT('Ctrl Pts',(-2.48421705019534,3.05156081249447,300.352701309249));
#8152=CARTESIAN_POINT('Ctrl Pts',(-2.38846261491229,3.12706454378054,300.34653031919));
#8153=CARTESIAN_POINT('Ctrl Pts',(-2.28955502976753,3.19787847887724,300.34035932913));
#8154=CARTESIAN_POINT('Ctrl Pts',(-2.19064744462277,3.26869241397394,300.334188339071));
#8155=CARTESIAN_POINT('Ctrl Pts',(-2.08858718539605,3.33481632871924,300.328017349011));
#8156=CARTESIAN_POINT('Ctrl Pts',(-1.98387193327471,3.39598898001228,300.321846358952));
#8157=CARTESIAN_POINT('Ctrl Pts',(-1.88406849122799,3.45429224562534,300.315964827501));
#8158=CARTESIAN_POINT('Ctrl Pts',(-1.78153192407064,3.50828608442161,300.31008329605));
#8159=CARTESIAN_POINT('Ctrl Pts',(-1.67667012221064,3.55770520157112,300.304201764598));
#8160=CARTESIAN_POINT('Ctrl Pts',(-1.57194084459013,3.60706186289017,300.298327666221));
#8161=CARTESIAN_POINT('Ctrl Pts',(-1.46489254604916,3.65185512709511,300.292453567843));
#8162=CARTESIAN_POINT('Ctrl Pts',(-1.35595994737082,3.69186424738588,300.286579469465));
#8163=CARTESIAN_POINT('Ctrl Pts',(-1.24713615661101,3.73183340434929,300.280711238463));
#8164=CARTESIAN_POINT('Ctrl Pts',(-1.13643219418239,3.76702778222883,300.27484300746));
#8165=CARTESIAN_POINT('Ctrl Pts',(-1.02430452134268,3.79727392316606,300.268974776457));
#8166=CARTESIAN_POINT('Ctrl Pts',(-0.910021548104855,3.82810145064198,300.262993747246));
#8167=CARTESIAN_POINT('Ctrl Pts',(-0.794259959272325,3.85378836150439,300.257012718035));
#8168=CARTESIAN_POINT('Ctrl Pts',(-0.677521633416676,3.87420358735217,300.251031688824));
#8169=CARTESIAN_POINT('Ctrl Pts',(-0.563110924343218,3.89421175903031,300.245169913884));
#8170=CARTESIAN_POINT('Ctrl Pts',(-0.447762491068235,3.90915644642779,300.239308138944));
#8171=CARTESIAN_POINT('Ctrl Pts',(-0.331960282241142,3.9189655996212,300.233446364005));
#8172=CARTESIAN_POINT('Ctrl Pts',(-0.216174088779671,3.92877339621549,300.227585399744));
#8173=CARTESIAN_POINT('Ctrl Pts',(-0.0999346547999836,3.93344703631298,
300.221724435484));
#8174=CARTESIAN_POINT('Ctrl Pts',(0.0162690097339698,3.93296635115561,300.215863471223));
#8175=CARTESIAN_POINT('Ctrl Pts',(0.132484480846329,3.93248561715945,300.210001911474));
#8176=CARTESIAN_POINT('Ctrl Pts',(0.24866376348413,3.92684951855367,300.204140351725));
#8177=CARTESIAN_POINT('Ctrl Pts',(0.364318601617826,3.91609000873515,300.198278791977));
#8178=CARTESIAN_POINT('Ctrl Pts',(0.484100520961988,3.90494655154769,300.192208065595));
#8179=CARTESIAN_POINT('Ctrl Pts',(0.603319392767887,3.88830724208551,300.186137339213));
#8180=CARTESIAN_POINT('Ctrl Pts',(0.721440848529659,3.8662659119715,300.18006661283));
#8181=CARTESIAN_POINT('Ctrl Pts',(0.835660540600444,3.84495264655145,300.174196413437));
#8182=CARTESIAN_POINT('Ctrl Pts',(0.948853777666821,3.81858875686659,300.168326214043));
#8183=CARTESIAN_POINT('Ctrl Pts',(1.06055093603876,3.78731048530053,300.162456014649));
#8184=CARTESIAN_POINT('Ctrl Pts',(1.1779714846907,3.75442950729085,300.156285024773));
#8185=CARTESIAN_POINT('Ctrl Pts',(1.29373807183774,3.71611734535367,300.150114034897));
#8186=CARTESIAN_POINT('Ctrl Pts',(1.40732806354347,3.67258992014668,300.143943045021));
#8187=CARTESIAN_POINT('Ctrl Pts',(1.5209180552492,3.62906249493968,300.137772055144));
#8188=CARTESIAN_POINT('Ctrl Pts',(1.63233100231152,3.58032008001792,300.131601065268));
#8189=CARTESIAN_POINT('Ctrl Pts',(1.74107469043959,3.52663407831188,300.125430075392));
#8190=CARTESIAN_POINT('Ctrl Pts',(1.84471761549434,3.47546628782131,300.119548543762));
#8191=CARTESIAN_POINT('Ctrl Pts',(1.94626996586553,3.41964332459357,300.113667012133));
#8192=CARTESIAN_POINT('Ctrl Pts',(2.04528561597544,3.35935942540895,300.107785480503));
#8193=CARTESIAN_POINT('Ctrl Pts',(2.14417613023306,3.29915171293921,300.101911381946));
#8194=CARTESIAN_POINT('Ctrl Pts',(2.24053597152125,3.23449448939036,300.096037283388));
#8195=CARTESIAN_POINT('Ctrl Pts',(2.33394140918747,3.16562892621356,300.090163184831));
#8196=CARTESIAN_POINT('Ctrl Pts',(2.42725354834476,3.09683214976397,300.084294953647));
#8197=CARTESIAN_POINT('Ctrl Pts',(2.51761682462389,3.02383563859343,300.078426722464));
#8198=CARTESIAN_POINT('Ctrl Pts',(2.60463499396856,2.94692476120351,300.07255849128));
#8199=CARTESIAN_POINT('Ctrl Pts',(2.69332580907198,2.86853551838904,300.066577462136));
#8200=CARTESIAN_POINT('Ctrl Pts',(2.77854121907186,2.78608009786493,300.060596432993));
#8201=CARTESIAN_POINT('Ctrl Pts',(2.85989533302364,2.69990512502747,300.054615403849));
#8202=CARTESIAN_POINT('Ctrl Pts',(2.93962735067599,2.61544837020939,300.048753628727));
#8203=CARTESIAN_POINT('Ctrl Pts',(3.01565032958605,2.52741932838689,300.042891853604));
#8204=CARTESIAN_POINT('Ctrl Pts',(3.08763751046008,2.43618217791688,300.037030078482));
#8205=CARTESIAN_POINT('Ctrl Pts',(3.15961473555994,2.34495764547769,300.031169114039));
#8206=CARTESIAN_POINT('Ctrl Pts',(3.22755701759814,2.25052620994329,300.025308149596));
#8207=CARTESIAN_POINT('Ctrl Pts',(3.29117810562532,2.15328485738708,300.019447185153));
#8208=CARTESIAN_POINT('Ctrl Pts',(3.35480565771185,2.05603362486979,300.013585625221));
#8209=CARTESIAN_POINT('Ctrl Pts',(3.41411091754167,1.95597225239564,300.00772406529));
#8210=CARTESIAN_POINT('Ctrl Pts',(3.46885154752756,1.85352581347433,300.001862505358));
#8211=CARTESIAN_POINT('Ctrl Pts',(3.5255455635491,1.74742363578561,299.995791779231));
#8212=CARTESIAN_POINT('Ctrl Pts',(3.57734286546249,1.63876341190897,299.989721053104));
#8213=CARTESIAN_POINT('Ctrl Pts',(3.62402734993076,1.52804278963446,299.983650326976));
#8214=CARTESIAN_POINT('Ctrl Pts',(3.66916976537472,1.42097946043933,299.977780127402));
#8215=CARTESIAN_POINT('Ctrl Pts',(3.70953171259698,1.31199011410391,299.971909927827));
#8216=CARTESIAN_POINT('Ctrl Pts',(3.7449681527168,1.20154173258232,299.966039728252));
#8217=CARTESIAN_POINT('Ctrl Pts',(3.78222036087105,1.08543396089785,299.959868738849));
#8218=CARTESIAN_POINT('Ctrl Pts',(3.8140287861813,0.967714182437371,299.953697749445));
#8219=CARTESIAN_POINT('Ctrl Pts',(3.84028567852364,0.848937516738543,299.947526760042));
#8220=CARTESIAN_POINT('Ctrl Pts',(3.86654257086599,0.73016085103972,299.941355770639));
#8221=CARTESIAN_POINT('Ctrl Pts',(3.8872479110456,0.610327823693746,299.935184781235));
#8222=CARTESIAN_POINT('Ctrl Pts',(3.90235701070326,0.489998735728107,299.929013791832));
#8223=CARTESIAN_POINT('Ctrl Pts',(3.92263821027235,0.328478969342776,299.920730368567));
#8224=CARTESIAN_POINT('Ctrl Pts',(3.93289389566743,0.165674836823054,299.912446945301));
#8225=CARTESIAN_POINT('Ctrl Pts',(3.93299918091997,0.00253828344068463,
299.904163522035));
#8226=CARTESIAN_POINT('',(3.93299999531041,0.000192063329847205,298.65416352207));
#8227=CARTESIAN_POINT('Ctrl Pts',(3.93299918092051,0.00253828261004938,
299.904163521993));
#8228=CARTESIAN_POINT('Ctrl Pts',(3.93307284838121,-0.111607424191687,299.898367658443));
#8229=CARTESIAN_POINT('Ctrl Pts',(3.92817312010893,-0.225939896070615,299.892571794893));
#8230=CARTESIAN_POINT('Ctrl Pts',(3.91827769750935,-0.339983654314229,299.886775931344));
#8231=CARTESIAN_POINT('Ctrl Pts',(3.90839302762208,-0.453903488621041,299.880986365782));
#8232=CARTESIAN_POINT('Ctrl Pts',(3.89352349123848,-0.567534813198981,299.87519680022));
#8233=CARTESIAN_POINT('Ctrl Pts',(3.87369882539846,-0.680401653515468,299.869407234658));
#8234=CARTESIAN_POINT('Ctrl Pts',(3.85389011836459,-0.793177636309329,299.863622329682));
#8235=CARTESIAN_POINT('Ctrl Pts',(3.82913428684059,-0.90518994231623,299.857837424706));
#8236=CARTESIAN_POINT('Ctrl Pts',(3.79951285333144,-1.01596804938404,299.85205251973));
#8237=CARTESIAN_POINT('Ctrl Pts',(3.76990412234892,-1.12669865159845,299.846270095489));
#8238=CARTESIAN_POINT('Ctrl Pts',(3.73543404440196,-1.23619569720181,299.840487671247));
#8239=CARTESIAN_POINT('Ctrl Pts',(3.69623502513004,-1.34399986570011,299.834705247006));
#8240=CARTESIAN_POINT('Ctrl Pts',(3.65704277323311,-1.45178542273193,299.82892382105));
#8241=CARTESIAN_POINT('Ctrl Pts',(3.61312334777438,-1.55787828487982,299.823142395094));
#8242=CARTESIAN_POINT('Ctrl Pts',(3.56465843411753,-1.66183610746511,299.817360969139));
#8243=CARTESIAN_POINT('Ctrl Pts',(3.51618947118613,-1.76580261579298,299.811579060141));
#8244=CARTESIAN_POINT('Ctrl Pts',(3.46317444555771,-1.86763334583981,299.805797151144));
#8245=CARTESIAN_POINT('Ctrl Pts',(3.40584204794065,-1.96690847384403,299.800015242147));
#8246=CARTESIAN_POINT('Ctrl Pts',(3.34845515127121,-2.06627797083725,299.79422783698));
#8247=CARTESIAN_POINT('Ctrl Pts',(3.28674289880943,-2.16308664588207,299.788440431813));
#8248=CARTESIAN_POINT('Ctrl Pts',(3.22097858646294,-2.25694172400335,299.782653026647));
#8249=CARTESIAN_POINT('Ctrl Pts',(3.15518287829366,-2.35084160845339,299.776862858578));
#8250=CARTESIAN_POINT('Ctrl Pts',(3.0853315172225,-2.44178475207879,299.771072690509));
#8251=CARTESIAN_POINT('Ctrl Pts',(3.01173836458176,-2.52941120091345,299.765282522441));
#8252=CARTESIAN_POINT('Ctrl Pts',(2.93802850167194,-2.61717661520962,299.759483171832));
#8253=CARTESIAN_POINT('Ctrl Pts',(2.86056528084323,-2.7016145152527,299.753683821223));
#8254=CARTESIAN_POINT('Ctrl Pts',(2.77969994058407,-2.78240134421994,299.747884470615));
#8255=CARTESIAN_POINT('Ctrl Pts',(2.70864684660833,-2.85338545350848,299.7427888165));
#8256=CARTESIAN_POINT('Ctrl Pts',(2.63496785311061,-2.92155124361669,299.737693162386));
#8257=CARTESIAN_POINT('Ctrl Pts',(2.55892100415829,-2.98670592701684,299.732597508272));
#8258=CARTESIAN_POINT('Ctrl Pts',(2.47114582301482,-3.06190909738593,299.726715976438));
#8259=CARTESIAN_POINT('Ctrl Pts',(2.37991126581068,-3.13336075403482,299.720834444605));
#8260=CARTESIAN_POINT('Ctrl Pts',(2.28557123593582,-3.20072696827811,299.714952912772));
#8261=CARTESIAN_POINT('Ctrl Pts',(2.19135043294819,-3.26800804513021,299.709078814016));
#8262=CARTESIAN_POINT('Ctrl Pts',(2.09403229515043,-3.33121371110383,299.70320471526));
#8263=CARTESIAN_POINT('Ctrl Pts',(1.99400508672333,-3.3900490725241,299.697330616504));
#8264=CARTESIAN_POINT('Ctrl Pts',(1.89407779108197,-3.44882566588563,299.691462385128));
#8265=CARTESIAN_POINT('Ctrl Pts',(1.79144716066328,-3.50324043080484,299.685594153751));
#8266=CARTESIAN_POINT('Ctrl Pts',(1.68653130241257,-3.5530411151551,299.679725922374));
#8267=CARTESIAN_POINT('Ctrl Pts',(1.57959877747443,-3.60379905594698,299.673744893305));
#8268=CARTESIAN_POINT('Ctrl Pts',(1.47029261830429,-3.64976344901614,299.667763864236));
#8269=CARTESIAN_POINT('Ctrl Pts',(1.35908319432061,-3.69071563127198,299.661782835166));
#8270=CARTESIAN_POINT('Ctrl Pts',(1.25009113839858,-3.73085128145942,299.655921059865));
#8271=CARTESIAN_POINT('Ctrl Pts',(1.13927141555826,-3.76617259484685,299.650059284564));
#8272=CARTESIAN_POINT('Ctrl Pts',(1.02708730306685,-3.79652218113879,299.644197509262));
#8273=CARTESIAN_POINT('Ctrl Pts',(0.914918705661378,-3.82686757007668,299.638336544646));
#8274=CARTESIAN_POINT('Ctrl Pts',(0.801386491275514,-3.85224249181793,299.632475580029));
#8275=CARTESIAN_POINT('Ctrl Pts',(0.686968190187093,-3.87253969710719,299.626614615412));
#8276=CARTESIAN_POINT('Ctrl Pts',(0.57253826402901,-3.89283896462272,299.620753055313));
#8277=CARTESIAN_POINT('Ctrl Pts',(0.457222477677544,-3.90805941818161,299.614891495214));
#8278=CARTESIAN_POINT('Ctrl Pts',(0.341506935893272,-3.91814522609063,299.609029935114));
#8279=CARTESIAN_POINT('Ctrl Pts',(0.221662164058092,-3.92859093916418,299.602959209248));
#8280=CARTESIAN_POINT('Ctrl Pts',(0.10138904847765,-3.93352866481383,299.596888483381));
#8281=CARTESIAN_POINT('Ctrl Pts',(-0.018769876342918,-3.93295521100127,
299.590817757514));
#8282=CARTESIAN_POINT('Ctrl Pts',(-0.134959752667976,-3.93240069931886,
299.584947557787));
#8283=CARTESIAN_POINT('Ctrl Pts',(-0.251042448199745,-3.92669342784198,
299.57907735806));
#8284=CARTESIAN_POINT('Ctrl Pts',(-0.366531549930758,-3.91588350476688,
299.573207158333));
#8285=CARTESIAN_POINT('Ctrl Pts',(-0.487938316693847,-3.90451968090961,
299.567036169396));
#8286=CARTESIAN_POINT('Ctrl Pts',(-0.608688522382004,-3.88751650818293,
299.560865180459));
#8287=CARTESIAN_POINT('Ctrl Pts',(-0.72822935608746,-3.86499301486205,299.554694191522));
#8288=CARTESIAN_POINT('Ctrl Pts',(-0.847770189792916,-3.84246952154117,
299.548523202586));
#8289=CARTESIAN_POINT('Ctrl Pts',(-0.966101160652827,-3.81442589648558,
299.542352213649));
#8290=CARTESIAN_POINT('Ctrl Pts',(-1.08268947065561,-3.78104119392152,299.536181224712));
#8291=CARTESIAN_POINT('Ctrl Pts',(-1.19380909825172,-3.74922243167823,299.530299691713));
#8292=CARTESIAN_POINT('Ctrl Pts',(-1.30370387739374,-3.71244979142711,299.524418158714));
#8293=CARTESIAN_POINT('Ctrl Pts',(-1.4119001488038,-3.67083464212266,299.518536625715));
#8294=CARTESIAN_POINT('Ctrl Pts',(-1.51995968209177,-3.62927208591862,299.51266252578));
#8295=CARTESIAN_POINT('Ctrl Pts',(-1.62632459580339,-3.58287933886022,299.506788425845));
#8296=CARTESIAN_POINT('Ctrl Pts',(-1.73053487590191,-3.53181795160611,299.50091432591));
#8297=CARTESIAN_POINT('Ctrl Pts',(-1.83464106516137,-3.48080756721503,299.495046093342));
#8298=CARTESIAN_POINT('Ctrl Pts',(-1.93659653428927,-3.42513799930513,299.489177860774));
#8299=CARTESIAN_POINT('Ctrl Pts',(-2.0359604134839,-3.36501919678424,299.483309628206));
#8300=CARTESIAN_POINT('Ctrl Pts',(-2.13723421255566,-3.30374482247153,299.477328599579));
#8301=CARTESIAN_POINT('Ctrl Pts',(-2.23581535812041,-3.23784856028069,299.471347570952));
#8302=CARTESIAN_POINT('Ctrl Pts',(-2.33126221818643,-3.16760247980337,299.465366542324));
#8303=CARTESIAN_POINT('Ctrl Pts',(-2.42480602102345,-3.09875699344899,299.45950476581));
#8304=CARTESIAN_POINT('Ctrl Pts',(-2.51533901974359,-3.0257337942245,299.453642989296));
#8305=CARTESIAN_POINT('Ctrl Pts',(-2.60247462395827,-2.94883279140294,299.447781212782));
#8306=CARTESIAN_POINT('Ctrl Pts',(-2.68959817738942,-2.87194242392783,299.441920246947));
#8307=CARTESIAN_POINT('Ctrl Pts',(-2.7733249620421,-2.79117559181146,299.436059281112));
#8308=CARTESIAN_POINT('Ctrl Pts',(-2.8533023795244,-2.70687172414956,299.430198315277));
#8309=CARTESIAN_POINT('Ctrl Pts',(-2.93328792288949,-2.62255929102794,299.424336753955));
#8310=CARTESIAN_POINT('Ctrl Pts',(-3.00952305837299,-2.53470940671756,299.418475192632));
#8311=CARTESIAN_POINT('Ctrl Pts',(-3.08169337346136,-2.44369698448157,299.41261363131));
#8312=CARTESIAN_POINT('Ctrl Pts',(-3.15643900057268,-2.34943689199591,299.40654290713));
#8313=CARTESIAN_POINT('Ctrl Pts',(-3.22682399373476,-2.25178471465513,299.40047218295));
#8314=CARTESIAN_POINT('Ctrl Pts',(-3.29254678082895,-2.15119145964578,299.39440145877));
#8315=CARTESIAN_POINT('Ctrl Pts',(-3.35609866619722,-2.05392091933815,299.388531257821));
#8316=CARTESIAN_POINT('Ctrl Pts',(-3.41529131848942,-1.9539009192602,299.382661056872));
#8317=CARTESIAN_POINT('Ctrl Pts',(-3.46989856633695,-1.85156499732869,299.376790855923));
#8318=CARTESIAN_POINT('Ctrl Pts',(-3.52730385002353,-1.743985456858,299.370619870127));
#8319=CARTESIAN_POINT('Ctrl Pts',(-3.5796411496913,-1.63384685421397,299.364448884332));
#8320=CARTESIAN_POINT('Ctrl Pts',(-3.62670522905839,-1.52167610926915,299.358277898537));
#8321=CARTESIAN_POINT('Ctrl Pts',(-3.67376930842548,-1.40950536432434,299.352106912741));
#8322=CARTESIAN_POINT('Ctrl Pts',(-3.7155600546627,-1.29530299077279,299.345935926946));
#8323=CARTESIAN_POINT('Ctrl Pts',(-3.75193335139576,-1.17961227811693,299.339764941151));
#8324=CARTESIAN_POINT('Ctrl Pts',(-3.78660050105938,-1.06934822149961,299.333883415214));
#8325=CARTESIAN_POINT('Ctrl Pts',(-3.816458629075,-0.95737701844418,299.328001889278));
#8326=CARTESIAN_POINT('Ctrl Pts',(-3.84133971506152,-0.844155313607069,
299.322120363341));
#8327=CARTESIAN_POINT('Ctrl Pts',(-3.86618935631761,-0.731076698424104,
299.31624627048));
#8328=CARTESIAN_POINT('Ctrl Pts',(-3.8860743777425,-0.616751123344073,299.310372177619));
#8329=CARTESIAN_POINT('Ctrl Pts',(-3.90087615535629,-0.501651493143109,
299.304498084758));
#8330=CARTESIAN_POINT('Ctrl Pts',(-3.91566314813149,-0.386666830853354,
299.298629859268));
#8331=CARTESIAN_POINT('Ctrl Pts',(-3.92537694518395,-0.270910057636561,
299.292761633778));
#8332=CARTESIAN_POINT('Ctrl Pts',(-3.92994986024603,-0.154864766658676,
299.286893408288));
#8333=CARTESIAN_POINT('Ctrl Pts',(-3.93461068114802,-0.03658871944896,299.280912377009));
#8334=CARTESIAN_POINT('Ctrl Pts',(-3.93393083611978,0.0819866281317321,
299.274931345729));
#8335=CARTESIAN_POINT('Ctrl Pts',(-3.92789406105627,0.200342818985095,299.26895031445));
#8336=CARTESIAN_POINT('Ctrl Pts',(-3.92197765932922,0.316338986575359,299.263088544976));
#8337=CARTESIAN_POINT('Ctrl Pts',(-3.91091600534963,0.432124226900779,299.257226775502));
#8338=CARTESIAN_POINT('Ctrl Pts',(-3.89474639354974,0.547210681485,299.251365006028));
#8339=CARTESIAN_POINT('Ctrl Pts',(-3.87857901792365,0.662281220206955,299.245504047207));
#8340=CARTESIAN_POINT('Ctrl Pts',(-3.85730514658442,0.776652757677666,299.239643088385));
#8341=CARTESIAN_POINT('Ctrl Pts',(-3.83101378264864,0.889844029679433,299.233782129564));
#8342=CARTESIAN_POINT('Ctrl Pts',(-3.80471974729484,1.00304680284201,299.227920575221));
#8343=CARTESIAN_POINT('Ctrl Pts',(-3.77340729903819,1.11506867100497,299.222059020878));
#8344=CARTESIAN_POINT('Ctrl Pts',(-3.73721609237713,1.22544068762116,299.216197466535));
#8345=CARTESIAN_POINT('Ctrl Pts',(-3.69973333972014,1.33975152112892,299.210126732456));
#8346=CARTESIAN_POINT('Ctrl Pts',(-3.65701725589882,1.45229209397296,299.204055998377));
#8347=CARTESIAN_POINT('Ctrl Pts',(-3.60927807499095,1.56256224752476,299.197985264299));
#8348=CARTESIAN_POINT('Ctrl Pts',(-3.56311590490991,1.66918974900922,299.192115070179));
#8349=CARTESIAN_POINT('Ctrl Pts',(-3.51225750028227,1.77369411483187,299.186244876059));
#8350=CARTESIAN_POINT('Ctrl Pts',(-3.45694005662018,1.87564774009804,299.180374681939));
#8351=CARTESIAN_POINT('Ctrl Pts',(-3.39878794744905,1.98282583717512,299.174203677881));
#8352=CARTESIAN_POINT('Ctrl Pts',(-3.33570797303367,2.08718439722229,299.168032673823));
#8353=CARTESIAN_POINT('Ctrl Pts',(-3.26802679801522,2.18826183247215,299.161861669765));
#8354=CARTESIAN_POINT('Ctrl Pts',(-3.20034562299678,2.28933926772201,299.155690665707));
#8355=CARTESIAN_POINT('Ctrl Pts',(-3.12806361391963,2.3871352009875,299.149519661649));
#8356=CARTESIAN_POINT('Ctrl Pts',(-3.05155477111898,2.48123003344329,299.143348657591));
#8357=CARTESIAN_POINT('Ctrl Pts',(-2.97863477264787,2.57091110542987,299.137467120373));
#8358=CARTESIAN_POINT('Ctrl Pts',(-2.90164055790344,2.65751939637476,299.131585583154));
#8359=CARTESIAN_POINT('Ctrl Pts',(-2.82086064564473,2.74066309820321,299.125704045936));
#8360=CARTESIAN_POINT('Ctrl Pts',(-2.74018282334396,2.82370172270753,299.119829941826));
#8361=CARTESIAN_POINT('Ctrl Pts',(-2.6557291034131,2.90328417357108,299.113955837717));
#8362=CARTESIAN_POINT('Ctrl Pts',(-2.56782878914213,2.97905090752959,299.108081733607));
#8363=CARTESIAN_POINT('Ctrl Pts',(-2.48001627511971,3.05474196100699,299.102213496914));
#8364=CARTESIAN_POINT('Ctrl Pts',(-2.38876432530163,3.12662461202969,299.096345260222));
#8365=CARTESIAN_POINT('Ctrl Pts',(-2.29443922687332,3.19437593814268,299.090477023529));
#8366=CARTESIAN_POINT('Ctrl Pts',(-2.19830115407132,3.2634294777712,299.084495996467));
#8367=CARTESIAN_POINT('Ctrl Pts',(-2.09897087987745,3.32819092747019,299.078514969405));
#8368=CARTESIAN_POINT('Ctrl Pts',(-1.99687211445838,3.38836107262767,299.072533942342));
#8369=CARTESIAN_POINT('Ctrl Pts',(-1.89680894051811,3.44733157708178,299.066672161851));
#8370=CARTESIAN_POINT('Ctrl Pts',(-1.79408701708441,3.50189194129735,299.06081038136));
#8371=CARTESIAN_POINT('Ctrl Pts',(-1.6891340297507,3.55180450328254,299.054948600869));
#8372=CARTESIAN_POINT('Ctrl Pts',(-1.58419555842818,3.60171016187864,299.049087631119));
#8373=CARTESIAN_POINT('Ctrl Pts',(-1.4770270086691,3.6469691198377,299.043226661369));
#8374=CARTESIAN_POINT('Ctrl Pts',(-1.36807905174343,3.68739050117841,299.037365691618));
#8375=CARTESIAN_POINT('Ctrl Pts',(-1.25912002669872,3.72781598896291,299.031504126447));
#8376=CARTESIAN_POINT('Ctrl Pts',(-1.14838162121822,3.76340277991293,299.025642561276));
#8377=CARTESIAN_POINT('Ctrl Pts',(-1.0363321333408,3.7940090549978,299.019780996105));
#8378=CARTESIAN_POINT('Ctrl Pts',(-0.920284477162809,3.82570742823645,299.013710277599));
#8379=CARTESIAN_POINT('Ctrl Pts',(-0.802830885538338,3.85206308744197,299.007639559092));
#8380=CARTESIAN_POINT('Ctrl Pts',(-0.684504583102838,3.87297591984655,299.001568840586));
#8381=CARTESIAN_POINT('Ctrl Pts',(-0.570086560908655,3.89319800802947,298.995698635987));
#8382=CARTESIAN_POINT('Ctrl Pts',(-0.45485299105735,3.90833114852157,298.989828431388));
#8383=CARTESIAN_POINT('Ctrl Pts',(-0.339291410563918,3.91833770095401,298.983958226788));
#8384=CARTESIAN_POINT('Ctrl Pts',(-0.217808817370258,3.92885695772802,298.977787251329));
#8385=CARTESIAN_POINT('Ctrl Pts',(-0.0959642399790542,3.93371035044302,
298.971616275869));
#8386=CARTESIAN_POINT('Ctrl Pts',(0.0256771420902181,3.93291618069519,298.96544530041));
#8387=CARTESIAN_POINT('Ctrl Pts',(0.147318524159488,3.93212201094737,298.95927432495));
#8388=CARTESIAN_POINT('Ctrl Pts',(0.268756194200433,3.92568037681522,298.953103349491));
#8389=CARTESIAN_POINT('Ctrl Pts',(0.38943393405726,3.91367221558023,298.946932374031));
#8390=CARTESIAN_POINT('Ctrl Pts',(0.504451614871845,3.90222726427658,298.941050831283));
#8391=CARTESIAN_POINT('Ctrl Pts',(0.61914961719036,3.8856892634248,298.935169288535));
#8392=CARTESIAN_POINT('Ctrl Pts',(0.733042001889961,3.86408312843618,298.929287745786));
#8393=CARTESIAN_POINT('Ctrl Pts',(0.846790451664222,3.84250429885025,298.923413636015));
#8394=CARTESIAN_POINT('Ctrl Pts',(0.959734907611862,3.81587014979798,298.917539526243));
#8395=CARTESIAN_POINT('Ctrl Pts',(1.07139388683557,3.78425740922197,298.911665416471));
#8396=CARTESIAN_POINT('Ctrl Pts',(1.18294133665201,3.75267624470229,298.905797173993));
#8397=CARTESIAN_POINT('Ctrl Pts',(1.2932054699101,3.71612649243231,298.899928931514));
#8398=CARTESIAN_POINT('Ctrl Pts',(1.4017149891287,3.67473592102234,298.894060689036));
#8399=CARTESIAN_POINT('Ctrl Pts',(1.51230996591828,3.63254985921544,298.888079664096));
#8400=CARTESIAN_POINT('Ctrl Pts',(1.62108176049001,3.58533506396183,298.882098639155));
#8401=CARTESIAN_POINT('Ctrl Pts',(1.72754722542983,3.53328028663304,298.876117614215));
#8402=CARTESIAN_POINT('Ctrl Pts',(1.83189018265554,3.48226327931258,298.870255827674));
#8403=CARTESIAN_POINT('Ctrl Pts',(1.9340175308548,3.42659767280112,298.864394041133));
#8404=CARTESIAN_POINT('Ctrl Pts',(2.03349529856749,3.36650944907391,298.858532254591));
#8405=CARTESIAN_POINT('Ctrl Pts',(2.13295930903918,3.30642953522531,298.852671278703));
#8406=CARTESIAN_POINT('Ctrl Pts',(2.22977411533169,3.24192843335955,298.846810302816));
#8407=CARTESIAN_POINT('Ctrl Pts',(2.32353212690091,3.17327708453884,298.840949326928));
#8408=CARTESIAN_POINT('Ctrl Pts',(2.41729966469621,3.10461876043935,298.835087755539));
#8409=CARTESIAN_POINT('Ctrl Pts',(2.50800945809351,3.03180959439804,298.829226184151));
#8410=CARTESIAN_POINT('Ctrl Pts',(2.59528514511845,2.95516226551564,298.823364612762));
#8411=CARTESIAN_POINT('Ctrl Pts',(2.68567479791148,2.87578018693958,298.817293902571));
#8412=CARTESIAN_POINT('Ctrl Pts',(2.77238035214324,2.7922812540297,298.81122319238));
#8413=CARTESIAN_POINT('Ctrl Pts',(2.85502448286709,2.7050553048375,298.805152482189));
#8414=CARTESIAN_POINT('Ctrl Pts',(2.93493910016204,2.62071019421887,298.799282271233));
#8415=CARTESIAN_POINT('Ctrl Pts',(3.01105610668511,2.53288072346202,298.793412060277));
#8416=CARTESIAN_POINT('Ctrl Pts',(3.08307548192846,2.441953024268,298.787541849322));
#8417=CARTESIAN_POINT('Ctrl Pts',(3.15878462992905,2.34636682107791,298.781370889513));
#8418=CARTESIAN_POINT('Ctrl Pts',(3.22996484918045,2.24735694818931,298.775199929705));
#8419=CARTESIAN_POINT('Ctrl Pts',(3.29632003099506,2.14540514897787,298.769028969896));
#8420=CARTESIAN_POINT('Ctrl Pts',(3.36267521280966,2.04345334976642,298.762858010088));
#8421=CARTESIAN_POINT('Ctrl Pts',(3.42420515436349,1.93856010947014,298.756687050279));
#8422=CARTESIAN_POINT('Ctrl Pts',(3.4806709553237,1.83123420150618,298.750516090471));
#8423=CARTESIAN_POINT('Ctrl Pts',(3.53742991076748,1.72335108775417,298.744313092783));
#8424=CARTESIAN_POINT('Ctrl Pts',(3.58923891626138,1.61269480481861,298.738110095095));
#8425=CARTESIAN_POINT('Ctrl Pts',(3.63583421788449,1.49973282289222,298.731907097407));
#8426=CARTESIAN_POINT('Ctrl Pts',(3.68450000718221,1.38175131360728,298.725428466129));
#8427=CARTESIAN_POINT('Ctrl Pts',(3.7274778434829,1.26125475726895,298.71894983485));
#8428=CARTESIAN_POINT('Ctrl Pts',(3.76451967885686,1.13880665062135,298.712471203572));
#8429=CARTESIAN_POINT('Ctrl Pts',(3.79983468351734,1.02206687751698,298.706294595652));
#8430=CARTESIAN_POINT('Ctrl Pts',(3.82975445226548,0.903553774660709,298.700117987731));
#8431=CARTESIAN_POINT('Ctrl Pts',(3.85411226710301,0.783777795402547,298.69394137981));
#8432=CARTESIAN_POINT('Ctrl Pts',(3.87843452805374,0.664176647164188,298.687773787575));
#8433=CARTESIAN_POINT('Ctrl Pts',(3.89721093602318,0.543316630173132,298.681606195341));
#8434=CARTESIAN_POINT('Ctrl Pts',(3.91032465648131,0.421722753612261,298.675438603106));
#8435=CARTESIAN_POINT('Ctrl Pts',(3.92341474746994,0.300347975728007,298.669282124188));
#8436=CARTESIAN_POINT('Ctrl Pts',(3.93086245247844,0.178242315916746,298.663125645271));
#8437=CARTESIAN_POINT('Ctrl Pts',(3.93260215939012,0.0559397529508584,298.656969166353));
#8438=CARTESIAN_POINT('Ctrl Pts',(3.9328664337595,0.037361087495771,298.656033951592));
#8439=CARTESIAN_POINT('Ctrl Pts',(3.93299908769365,0.0187778949398582,298.655098736831));
#8440=CARTESIAN_POINT('Ctrl Pts',(3.93299999531041,0.00019206332985904,
298.65416352207));
#8441=CARTESIAN_POINT('',(3.93299891020702,-0.00292785080898043,297.404163522073));
#8442=CARTESIAN_POINT('Ctrl Pts',(3.93299999531044,0.000192062627323755,
298.654163522035));
#8443=CARTESIAN_POINT('Ctrl Pts',(3.93300592546174,-0.121243769823802,298.648053029623));
#8444=CARTESIAN_POINT('Ctrl Pts',(3.92738333505017,-0.242584282912523,298.641942537212));
#8445=CARTESIAN_POINT('Ctrl Pts',(3.91618452274351,-0.363301230144049,298.6358320448));
#8446=CARTESIAN_POINT('Ctrl Pts',(3.90497215809457,-0.484164264062538,298.629714157721));
#8447=CARTESIAN_POINT('Ctrl Pts',(3.88817014637699,-0.604401871430454,298.623596270643));
#8448=CARTESIAN_POINT('Ctrl Pts',(3.86588221445863,-0.723494093916756,298.617478383565));
#8449=CARTESIAN_POINT('Ctrl Pts',(3.84354528529558,-0.842848125833726,298.611347047073));
#8450=CARTESIAN_POINT('Ctrl Pts',(3.81569839813161,-0.961051387962721,298.605215710581));
#8451=CARTESIAN_POINT('Ctrl Pts',(3.78249599553529,-1.07759595570858,298.599084374089));
#8452=CARTESIAN_POINT('Ctrl Pts',(3.74925373452515,-1.19428043145043,298.592945677126));
#8453=CARTESIAN_POINT('Ctrl Pts',(3.71064324573644,-1.3093019018455,298.586806980162));
#8454=CARTESIAN_POINT('Ctrl Pts',(3.66686763707445,-1.42217113322414,298.580668283198));
#8455=CARTESIAN_POINT('Ctrl Pts',(3.62299912652175,-1.53527989902203,298.574516558511));
#8456=CARTESIAN_POINT('Ctrl Pts',(3.57394373112134,-1.6462269692045,298.568364833823));
#8457=CARTESIAN_POINT('Ctrl Pts',(3.51995162947914,-1.75454539015871,298.562213109135));
#8458=CARTESIAN_POINT('Ctrl Pts',(3.49621550882068,-1.8021645609467,298.55950867506));
#8459=CARTESIAN_POINT('Ctrl Pts',(3.47152586032443,-1.84927605671103,298.556804240986));
#8460=CARTESIAN_POINT('Ctrl Pts',(3.44590658279842,-1.89584198250447,298.554099806911));
#8461=CARTESIAN_POINT('Ctrl Pts',(3.39018977189996,-1.99711356907094,298.548218203037));
#8462=CARTESIAN_POINT('Ctrl Pts',(3.32991504275857,-2.09609001452669,298.542336599164));
#8463=CARTESIAN_POINT('Ctrl Pts',(3.26529624385002,-2.1923342445665,298.536454995291));
#8464=CARTESIAN_POINT('Ctrl Pts',(3.2007591122629,-2.28845683804536,298.530580824778));
#8465=CARTESIAN_POINT('Ctrl Pts',(3.1318890575964,-2.38185374478624,298.524706654265));
#8466=CARTESIAN_POINT('Ctrl Pts',(3.05894582285887,-2.47211234631727,298.518832483753));
#8467=CARTESIAN_POINT('Ctrl Pts',(2.98607545158111,-2.56228078795882,298.512964180986));
#8468=CARTESIAN_POINT('Ctrl Pts',(2.90914025137754,-2.64931684198198,298.50709587822));
#8469=CARTESIAN_POINT('Ctrl Pts',(2.82844289897526,-2.73283731078827,298.501227575453));
#8470=CARTESIAN_POINT('Ctrl Pts',(2.74619577248773,-2.81796177098077,298.495246573282));
#8471=CARTESIAN_POINT('Ctrl Pts',(2.66004074138595,-2.89943385882113,298.489265571111));
#8472=CARTESIAN_POINT('Ctrl Pts',(2.57034120142409,-2.97688345560618,298.48328456894));
#8473=CARTESIAN_POINT('Ctrl Pts',(2.48242870531812,-3.05279005867983,298.477422723603));
#8474=CARTESIAN_POINT('Ctrl Pts',(2.3911119504255,-3.12483268317989,298.471560878266));
#8475=CARTESIAN_POINT('Ctrl Pts',(2.29676926178821,-3.19270104427346,298.465699032929));
#8476=CARTESIAN_POINT('Ctrl Pts',(2.20243963070255,-3.26056001200925,298.459837998904));
#8477=CARTESIAN_POINT('Ctrl Pts',(2.10508523294911,-3.32424562487915,298.453976964878));
#8478=CARTESIAN_POINT('Ctrl Pts',(2.00511537172842,-3.38348952208491,298.448115930853));
#8479=CARTESIAN_POINT('Ctrl Pts',(1.90513536553249,-3.44273943138134,298.442254302048));
#8480=CARTESIAN_POINT('Ctrl Pts',(1.80253972250091,-3.49754651902391,298.436392673244));
#8481=CARTESIAN_POINT('Ctrl Pts',(1.69776385742003,-3.54768754041816,298.430531044439));
#8482=CARTESIAN_POINT('Ctrl Pts',(1.58925218067232,-3.59961635342422,298.424460417681));
#8483=CARTESIAN_POINT('Ctrl Pts',(1.47840233594215,-3.64653994187821,298.418389790924));
#8484=CARTESIAN_POINT('Ctrl Pts',(1.36572103526904,-3.68826450431957,298.412319164166));
#8485=CARTESIAN_POINT('Ctrl Pts',(1.25675877473323,-3.72861194987016,298.406448898112));
#8486=CARTESIAN_POINT('Ctrl Pts',(1.14608446214156,-3.76409807287149,298.400578632057));
#8487=CARTESIAN_POINT('Ctrl Pts',(1.03417106279053,-3.79459868930651,298.394708366002));
#8488=CARTESIAN_POINT('Ctrl Pts',(0.916528013255468,-3.82666085121851,298.388537558893));
#8489=CARTESIAN_POINT('Ctrl Pts',(0.797516160316329,-3.85321339277487,298.382366751785));
#8490=CARTESIAN_POINT('Ctrl Pts',(0.677694799480092,-3.87417330004191,298.376195944676));
#8491=CARTESIAN_POINT('Ctrl Pts',(0.557873438643857,-3.89513320730896,298.370025137567));
#8492=CARTESIAN_POINT('Ctrl Pts',(0.437243095715267,-3.91050048441079,298.363854330459));
#8493=CARTESIAN_POINT('Ctrl Pts',(0.316365446062836,-3.92025533665059,298.35768352335));
#8494=CARTESIAN_POINT('Ctrl Pts',(0.201152958180538,-3.92955300912109,298.351801922895));
#8495=CARTESIAN_POINT('Ctrl Pts',(0.0853446993142111,-3.93378238818516,
298.345920322439));
#8496=CARTESIAN_POINT('Ctrl Pts',(-0.0305767527499009,-3.9328811401047,
298.340038721984));
#8497=CARTESIAN_POINT('Ctrl Pts',(-0.146351724133139,-3.93198103085947,
298.334164553637));
#8498=CARTESIAN_POINT('Ctrl Pts',(-0.262239196010664,-3.92596319167233,
298.328290385291));
#8499=CARTESIAN_POINT('Ctrl Pts',(-0.377751715330621,-3.91481706361418,
298.322416216944));
#8500=CARTESIAN_POINT('Ctrl Pts',(-0.493148872743679,-3.90368206715107,
298.316547915107));
#8501=CARTESIAN_POINT('Ctrl Pts',(-0.608171414906144,-3.88742900935181,
298.31067961327));
#8502=CARTESIAN_POINT('Ctrl Pts',(-0.722332788267097,-3.86609937055351,
298.304811311433));
#8503=CARTESIAN_POINT('Ctrl Pts',(-0.838686638799827,-3.84436009454808,
298.298830308447));
#8504=CARTESIAN_POINT('Ctrl Pts',(-0.954145466794198,-3.81734723524644,
298.292849305462));
#8505=CARTESIAN_POINT('Ctrl Pts',(-1.06820018125089,-3.78516015153594,298.286868302477));
#8506=CARTESIAN_POINT('Ctrl Pts',(-1.17998265929118,-3.75361430974246,298.281006455047));
#8507=CARTESIAN_POINT('Ctrl Pts',(-1.29041603865742,-3.71709861804354,298.275144607617));
#8508=CARTESIAN_POINT('Ctrl Pts',(-1.39903293763322,-3.67575785919276,298.269282760187));
#8509=CARTESIAN_POINT('Ctrl Pts',(-1.50763482412505,-3.6344228142547,298.263421722952));
#8510=CARTESIAN_POINT('Ctrl Pts',(-1.61442034475976,-3.58826417486692,298.257560685717));
#8511=CARTESIAN_POINT('Ctrl Pts',(-1.71894003852442,-3.53747567397398,298.251699648482));
#8512=CARTESIAN_POINT('Ctrl Pts',(-1.82347035873041,-3.48668200945105,298.245838015359));
#8513=CARTESIAN_POINT('Ctrl Pts',(-1.92573402373538,-3.43125772765636,298.239976382237));
#8514=CARTESIAN_POINT('Ctrl Pts',(-2.02530483839693,-3.37144320900797,298.234114749114));
#8515=CARTESIAN_POINT('Ctrl Pts',(-2.12842578464202,-3.30949604323273,298.228044123337));
#8516=CARTESIAN_POINT('Ctrl Pts',(-2.22865786308579,-3.24283997869521,298.22197349756));
#8517=CARTESIAN_POINT('Ctrl Pts',(-2.32556017139335,-3.17179111689735,298.215902871783));
#8518=CARTESIAN_POINT('Ctrl Pts',(-2.41926435143361,-3.10308712569383,298.210032598714));
#8519=CARTESIAN_POINT('Ctrl Pts',(-2.50985479538895,-3.03027602921799,298.204162325646));
#8520=CARTESIAN_POINT('Ctrl Pts',(-2.59696729089442,-2.95368412157165,298.198292052577));
#8521=CARTESIAN_POINT('Ctrl Pts',(-2.68853951702541,-2.87317108557035,298.192121250446));
#8522=CARTESIAN_POINT('Ctrl Pts',(-2.77626788162017,-2.78848024315026,298.185950448315));
#8523=CARTESIAN_POINT('Ctrl Pts',(-2.859774970519,-2.70003261424618,298.179779646183));
#8524=CARTESIAN_POINT('Ctrl Pts',(-2.94328205941782,-2.6115849853421,298.173608844052));
#8525=CARTESIAN_POINT('Ctrl Pts',(-3.02256758638687,-2.51938101103282,298.167438041921));
#8526=CARTESIAN_POINT('Ctrl Pts',(-3.09730558529359,-2.42387852651677,298.16126723979));
#8527=CARTESIAN_POINT('Ctrl Pts',(-3.16853413426333,-2.33286052369905,298.155386198175));
#8528=CARTESIAN_POINT('Ctrl Pts',(-3.23586214076153,-2.23855339493931,298.149505156561));
#8529=CARTESIAN_POINT('Ctrl Pts',(-3.29897171895252,-2.1413254300903,298.143624114946));
#8530=CARTESIAN_POINT('Ctrl Pts',(-3.36200152243356,-2.04422036786429,298.137750507359));
#8531=CARTESIAN_POINT('Ctrl Pts',(-3.42082328052744,-1.9442021551057,298.131876899773));
#8532=CARTESIAN_POINT('Ctrl Pts',(-3.4751596251509,-1.8416716807621,298.126003292186));
#8533=CARTESIAN_POINT('Ctrl Pts',(-3.52944168790985,-1.73924363409106,298.120135552318));
#8534=CARTESIAN_POINT('Ctrl Pts',(-3.57924705908134,-1.63430868024482,298.11426781245));
#8535=CARTESIAN_POINT('Ctrl Pts',(-3.6243422919032,-1.52729563317711,298.108400072582));
#8536=CARTESIAN_POINT('Ctrl Pts',(-3.67030959908303,-1.41821311382871,298.1024188594));
#8537=CARTESIAN_POINT('Ctrl Pts',(-3.71138246354779,-1.30697165608777,298.096437646219));
#8538=CARTESIAN_POINT('Ctrl Pts',(-3.74736324720497,-1.19405095933861,298.090456433038));
#8539=CARTESIAN_POINT('Ctrl Pts',(-3.78262259370264,-1.0833943930066,298.084595146912));
#8540=CARTESIAN_POINT('Ctrl Pts',(-3.81299202521437,-0.971125709909917,
298.078733860787));
#8541=CARTESIAN_POINT('Ctrl Pts',(-3.83833487108371,-0.857714648016914,
298.072872574661));
#8542=CARTESIAN_POINT('Ctrl Pts',(-3.8636742192528,-0.744319238584625,298.067012097483));
#8543=CARTESIAN_POINT('Ctrl Pts',(-3.88398827162279,-0.629782165769389,
298.061151620304));
#8544=CARTESIAN_POINT('Ctrl Pts',(-3.89919108151134,-0.514585182319152,
298.055291143126));
#8545=CARTESIAN_POINT('Ctrl Pts',(-3.91439544207652,-0.399376448852254,
298.049430068182));
#8546=CARTESIAN_POINT('Ctrl Pts',(-3.92448746988109,-0.283508079287484,
298.043568993239));
#8547=CARTESIAN_POINT('Ctrl Pts',(-3.92943296570268,-0.16746811054364,298.037707918296));
#8548=CARTESIAN_POINT('Ctrl Pts',(-3.93455594236022,-0.0472637725635806,
298.03163650479));
#8549=CARTESIAN_POINT('Ctrl Pts',(-3.93415603527685,0.0731242358104111,
298.025565091285));
#8550=CARTESIAN_POINT('Ctrl Pts',(-3.92825415593846,0.193153530519733,298.019493677779));
#8551=CARTESIAN_POINT('Ctrl Pts',(-3.92254833354875,0.309195522892783,298.013623953047));
#8552=CARTESIAN_POINT('Ctrl Pts',(-3.91170037762075,0.42490184480052,298.007754228316));
#8553=CARTESIAN_POINT('Ctrl Pts',(-3.89578194842871,0.539788857144138,298.001884503584));
#8554=CARTESIAN_POINT('Ctrl Pts',(-3.87904306292674,0.660597293836267,297.995712245691));
#8555=CARTESIAN_POINT('Ctrl Pts',(-3.85669719999763,0.780499192984246,297.989539987799));
#8556=CARTESIAN_POINT('Ctrl Pts',(-3.82888795165656,0.898947191807865,297.983367729907));
#8557=CARTESIAN_POINT('Ctrl Pts',(-3.80107870331549,1.01739519063148,297.977195472014));
#8558=CARTESIAN_POINT('Ctrl Pts',(-3.76780628045255,1.13438880639514,297.971023214122));
#8559=CARTESIAN_POINT('Ctrl Pts',(-3.7292734174472,1.24940336878114,297.96485095623));
#8560=CARTESIAN_POINT('Ctrl Pts',(-3.69255030673762,1.35901610394514,297.958968587461));
#8561=CARTESIAN_POINT('Ctrl Pts',(-3.6509313368372,1.46718474982083,297.953086218692));
#8562=CARTESIAN_POINT('Ctrl Pts',(-3.60454886705646,1.57344096330368,297.947203849924));
#8563=CARTESIAN_POINT('Ctrl Pts',(-3.55822502384188,1.67956287093865,297.941328916358));
#8564=CARTESIAN_POINT('Ctrl Pts',(-3.50714981889474,1.78377677975772,297.935453982793));
#8565=CARTESIAN_POINT('Ctrl Pts',(-3.45150513642287,1.88563021116193,297.929579049227));
#8566=CARTESIAN_POINT('Ctrl Pts',(-3.39591605660351,1.98738186606743,297.923709986158));
#8567=CARTESIAN_POINT('Ctrl Pts',(-3.33576677859773,2.08677737638179,297.917840923088));
#8568=CARTESIAN_POINT('Ctrl Pts',(-3.27128668580881,2.18338554067988,297.911971860019));
#8569=CARTESIAN_POINT('Ctrl Pts',(-3.2055799235782,2.28183157893004,297.905991143879));
#8570=CARTESIAN_POINT('Ctrl Pts',(-3.13537605516695,2.37738273490431,297.900010427739));
#8571=CARTESIAN_POINT('Ctrl Pts',(-3.06096638708415,2.46961004556206,297.8940297116));
#8572=CARTESIAN_POINT('Ctrl Pts',(-2.98802634681497,2.56001582113692,297.888167117567));
#8573=CARTESIAN_POINT('Ctrl Pts',(-2.91104538687808,2.64722750833493,297.882304523535));
#8574=CARTESIAN_POINT('Ctrl Pts',(-2.83034034309815,2.7308721211787,297.876441929502));
#8575=CARTESIAN_POINT('Ctrl Pts',(-2.74964654562697,2.81450507808255,297.870580152427));
#8576=CARTESIAN_POINT('Ctrl Pts',(-2.6652299821397,2.89457165299403,297.864718375351));
#8577=CARTESIAN_POINT('Ctrl Pts',(-2.57744546206122,2.97073457079222,297.858856598276));
#8578=CARTESIAN_POINT('Ctrl Pts',(-2.48965213151049,3.04690513266334,297.852994232884));
#8579=CARTESIAN_POINT('Ctrl Pts',(-2.39849048336277,3.11917098878944,297.847131867493));
#8580=CARTESIAN_POINT('Ctrl Pts',(-2.30434908434721,3.18723458463104,297.841269502102));
#8581=CARTESIAN_POINT('Ctrl Pts',(-2.20688028290387,3.25770386996115,297.835199932982));
#8582=CARTESIAN_POINT('Ctrl Pts',(-2.10621757909698,3.32366806059187,297.829130363863));
#8583=CARTESIAN_POINT('Ctrl Pts',(-2.00282454310868,3.38484605994446,297.823060794743));
#8584=CARTESIAN_POINT('Ctrl Pts',(-1.90281440835841,3.44402238551146,297.817189814946));
#8585=CARTESIAN_POINT('Ctrl Pts',(-1.8002502124232,3.49872067762816,297.811318835148));
#8586=CARTESIAN_POINT('Ctrl Pts',(-1.69557517532176,3.54873411582674,297.80544785535));
#8587=CARTESIAN_POINT('Ctrl Pts',(-1.58558909679209,3.60128515467582,297.79927899157));
#8588=CARTESIAN_POINT('Ctrl Pts',(-1.47327284269019,3.64866325818106,297.79311012779));
#8589=CARTESIAN_POINT('Ctrl Pts',(-1.35916125131522,3.69068688632932,297.78694126401));
#8590=CARTESIAN_POINT('Ctrl Pts',(-1.24504965994025,3.73271051447759,297.780772400229));
#8591=CARTESIAN_POINT('Ctrl Pts',(-1.12914324806311,3.76937957736814,297.774603536449));
#8592=CARTESIAN_POINT('Ctrl Pts',(-1.0119904910506,3.80057419951554,297.768434672669));
#8593=CARTESIAN_POINT('Ctrl Pts',(-0.900289521454252,3.83031715758936,297.762552881381));
#8594=CARTESIAN_POINT('Ctrl Pts',(-0.787096555945675,3.85517935855739,297.756671090093));
#8595=CARTESIAN_POINT('Ctrl Pts',(-0.672875318114343,3.87501326530278,297.750789298805));
#8596=CARTESIAN_POINT('Ctrl Pts',(-0.558798247404457,3.89482213819898,297.744914931363));
#8597=CARTESIAN_POINT('Ctrl Pts',(-0.443695887817354,3.90961526946071,297.739040563922));
#8598=CARTESIAN_POINT('Ctrl Pts',(-0.328046006161694,3.91929519401657,297.73316619648));
#8599=CARTESIAN_POINT('Ctrl Pts',(-0.212511464138736,3.92896546461578,297.727297687647));
#8600=CARTESIAN_POINT('Ctrl Pts',(-0.0964308943236152,3.93353263860112,
297.721429178814));
#8601=CARTESIAN_POINT('Ctrl Pts',(0.0197095274428665,3.93295061430066,297.715560669981));
#8602=CARTESIAN_POINT('Ctrl Pts',(0.138074782256221,3.93235744050653,297.709579741611));
#8603=CARTESIAN_POINT('Ctrl Pts',(0.256501777629808,3.92641568171508,297.703598813241));
#8604=CARTESIAN_POINT('Ctrl Pts',(0.374471899212748,3.91513215571326,297.697617884872));
#8605=CARTESIAN_POINT('Ctrl Pts',(0.490097659054271,3.90407286162977,297.691755812526));
#8606=CARTESIAN_POINT('Ctrl Pts',(0.605284107964331,3.88788219072501,297.685893740181));
#8607=CARTESIAN_POINT('Ctrl Pts',(0.719545481487535,3.8666191046017,297.680031667836));
#8608=CARTESIAN_POINT('Ctrl Pts',(0.833791184565131,3.84535893461728,297.674170399448));
#8609=CARTESIAN_POINT('Ctrl Pts',(0.947111659863042,3.81902780818591,297.66830913106));
#8610=CARTESIAN_POINT('Ctrl Pts',(1.05903003137945,3.78773605107806,297.662447862673));
#8611=CARTESIAN_POINT('Ctrl Pts',(1.17095989457509,3.75644108096032,297.656585992455));
#8612=CARTESIAN_POINT('Ctrl Pts',(1.28148697124422,3.72018457847325,297.650724122237));
#8613=CARTESIAN_POINT('Ctrl Pts',(1.3901489438384,3.67912692278276,297.64486225202));
#8614=CARTESIAN_POINT('Ctrl Pts',(1.50267500266412,3.63660923173433,297.63879193011));
#8615=CARTESIAN_POINT('Ctrl Pts',(1.61320039289943,3.5889427325439,297.632721608201));
#8616=CARTESIAN_POINT('Ctrl Pts',(1.72123492817387,3.53635961435404,297.626651286292));
#8617=CARTESIAN_POINT('Ctrl Pts',(1.82571360206621,3.4855072230919,297.620780763671));
#8618=CARTESIAN_POINT('Ctrl Pts',(1.92786247186775,3.43005702704061,297.61491024105));
#8619=CARTESIAN_POINT('Ctrl Pts',(2.0272648534531,3.37026500648744,297.609039718429));
#8620=CARTESIAN_POINT('Ctrl Pts',(2.13174187482091,3.30742051413899,297.602869496876));
#8621=CARTESIAN_POINT('Ctrl Pts',(2.23318414193663,3.23977947730182,297.596699275322));
#8622=CARTESIAN_POINT('Ctrl Pts',(2.33114523187613,3.16768857495512,297.590529053769));
#8623=CARTESIAN_POINT('Ctrl Pts',(2.42910632181563,3.09559767260841,297.584358832216));
#8624=CARTESIAN_POINT('Ctrl Pts',(2.52358587443011,3.01905728729746,297.578188610662));
#8625=CARTESIAN_POINT('Ctrl Pts',(2.61418148415182,2.93845948890193,297.572018389109));
#8626=CARTESIAN_POINT('Ctrl Pts',(2.69924849442303,2.86278017325948,297.566224705487));
#8627=CARTESIAN_POINT('Ctrl Pts',(2.7811840106951,2.7832633871791,297.560431021865));
#8628=CARTESIAN_POINT('Ctrl Pts',(2.85961492825546,2.70020211504593,297.554637338244));
#8629=CARTESIAN_POINT('Ctrl Pts',(2.93794564118625,2.61724696335945,297.548851056727));
#8630=CARTESIAN_POINT('Ctrl Pts',(3.01278036575709,2.53075663294805,297.543064775211));
#8631=CARTESIAN_POINT('Ctrl Pts',(3.08377951424885,2.44106388845092,297.537278493694));
#8632=CARTESIAN_POINT('Ctrl Pts',(3.15470070274579,2.35146963028841,297.531498565754));
#8633=CARTESIAN_POINT('Ctrl Pts',(3.22179443066285,2.25868028457932,297.525718637813));
#8634=CARTESIAN_POINT('Ctrl Pts',(3.28475908251103,2.16306420844628,297.519938709873));
#8635=CARTESIAN_POINT('Ctrl Pts',(3.34768560904992,2.06750602817017,297.514162281698));
#8636=CARTESIAN_POINT('Ctrl Pts',(3.40648779386134,1.96912487228284,297.508385853524));
#8637=CARTESIAN_POINT('Ctrl Pts',(3.46090566195918,1.86832036841086,297.502609425349));
#8638=CARTESIAN_POINT('Ctrl Pts',(3.51530458690881,1.76755095512078,297.49683500798));
#8639=CARTESIAN_POINT('Ctrl Pts',(3.56532202691158,1.66436024449566,297.49106059061));
#8640=CARTESIAN_POINT('Ctrl Pts',(3.61074299468598,1.55917414881281,297.485286173241));
#8641=CARTESIAN_POINT('Ctrl Pts',(3.65615984121502,1.45399759712978,297.47951227981));
#8642=CARTESIAN_POINT('Ctrl Pts',(3.69698087751575,1.34682641140872,297.473738386379));
#8643=CARTESIAN_POINT('Ctrl Pts',(3.73303883802,1.23810744034365,297.467964492948));
#8644=CARTESIAN_POINT('Ctrl Pts',(3.76911983671521,1.1293190064365,297.462186910455));
#8645=CARTESIAN_POINT('Ctrl Pts',(3.80043154588862,1.01898121590954,297.456409327962));
#8646=CARTESIAN_POINT('Ctrl Pts',(3.82685634873196,0.90755687765004,297.450631745468));
#8647=CARTESIAN_POINT('Ctrl Pts',(3.85328991848953,0.796095572317501,297.444852246156));
#8648=CARTESIAN_POINT('Ctrl Pts',(3.87483327108257,0.683547418900585,297.439072746844));
#8649=CARTESIAN_POINT('Ctrl Pts',(3.8914201055522,0.570384573865847,297.433293247531));
#8650=CARTESIAN_POINT('Ctrl Pts',(3.90802739377755,0.45708218411007,297.427506621334));
#8651=CARTESIAN_POINT('Ctrl Pts',(3.91966591310782,0.343164012069071,297.421719995136));
#8652=CARTESIAN_POINT('Ctrl Pts',(3.92632133292992,0.229106504882301,297.415933368938));
#8653=CARTESIAN_POINT('Ctrl Pts',(3.93083364974762,0.151776505931063,297.41201008665));
#8654=CARTESIAN_POINT('Ctrl Pts',(3.93305646252219,0.0743825067181312,297.408086804362));
#8655=CARTESIAN_POINT('Ctrl Pts',(3.93299891020702,-0.00292785080896812,
297.404163522073));
#8656=CARTESIAN_POINT('',(-1.75029459251059,-3.52206726787383,297.));
#8657=CARTESIAN_POINT('Ctrl Pts',(3.93299891020646,-0.00292785156004575,
297.404163522035));
#8658=CARTESIAN_POINT('Ctrl Pts',(3.93285925027004,-0.190533803048494,297.394643049873));
#8659=CARTESIAN_POINT('Ctrl Pts',(3.91929411197807,-0.37765441708386,297.385122577711));
#8660=CARTESIAN_POINT('Ctrl Pts',(3.89252247461753,-0.56281238845409,297.375602105549));
#8661=CARTESIAN_POINT('Ctrl Pts',(3.87595824961153,-0.677373864770567,297.369711571439));
#8662=CARTESIAN_POINT('Ctrl Pts',(3.85430595318971,-0.791385302525627,297.363821037329));
#8663=CARTESIAN_POINT('Ctrl Pts',(3.82761280904807,-0.904361202181478,297.357930503219));
#8664=CARTESIAN_POINT('Ctrl Pts',(3.80095340004707,-1.01719432143485,297.352047413642));
#8665=CARTESIAN_POINT('Ctrl Pts',(3.76926590808212,-1.12899410958632,297.346164324065));
#8666=CARTESIAN_POINT('Ctrl Pts',(3.73264911103967,-1.23928189442707,297.340281234488));
#8667=CARTESIAN_POINT('Ctrl Pts',(3.69606897287334,-1.34945926474311,297.334404034761));
#8668=CARTESIAN_POINT('Ctrl Pts',(3.65456947581911,-1.45812725580961,297.328526835035));
#8669=CARTESIAN_POINT('Ctrl Pts',(3.60829992222045,-1.56481969290519,297.322649635308));
#8670=CARTESIAN_POINT('Ctrl Pts',(3.56123948167204,-1.67333582721792,297.31667197642));
#8671=CARTESIAN_POINT('Ctrl Pts',(3.50924450677633,-1.77980782725634,297.310694317531));
#8672=CARTESIAN_POINT('Ctrl Pts',(3.45252441188082,-1.8837633039655,297.304716658643));
#8673=CARTESIAN_POINT('Ctrl Pts',(3.39681987633037,-1.98585748343887,297.298846028267));
#8674=CARTESIAN_POINT('Ctrl Pts',(3.33655823173306,-2.0855241361153,297.29297539789));
#8675=CARTESIAN_POINT('Ctrl Pts',(3.27198511558443,-2.18233874625228,297.287104767514));
#8676=CARTESIAN_POINT('Ctrl Pts',(3.20742155668761,-2.27913902718131,297.28123500603));
#8677=CARTESIAN_POINT('Ctrl Pts',(3.13854802308323,-2.37308776380244,297.275365244546));
#8678=CARTESIAN_POINT('Ctrl Pts',(3.06565390023675,-2.46378878233569,297.269495483062));
#8679=CARTESIAN_POINT('Ctrl Pts',(2.99275322829802,-2.55449794980214,297.263625194215));
#8680=CARTESIAN_POINT('Ctrl Pts',(2.91583150616474,-2.64195849925863,297.257754905369));
#8681=CARTESIAN_POINT('Ctrl Pts',(2.83521844734992,-2.72580728515549,297.251884616523));
#8682=CARTESIAN_POINT('Ctrl Pts',(2.75202446898228,-2.81234058611954,297.245826383645));
#8683=CARTESIAN_POINT('Ctrl Pts',(2.66489913319049,-2.89502662274155,297.239768150767));
#8684=CARTESIAN_POINT('Ctrl Pts',(2.57424503439676,-2.97350828195982,297.233709917889));
#8685=CARTESIAN_POINT('Ctrl Pts',(2.48627774869555,-3.04966389577787,297.227831239379));
#8686=CARTESIAN_POINT('Ctrl Pts',(2.39498828486449,-3.12186062420929,297.22195256087));
#8687=CARTESIAN_POINT('Ctrl Pts',(2.30077631500182,-3.18981462601303,297.21607388236));
#8688=CARTESIAN_POINT('Ctrl Pts',(2.20224802540595,-3.26088193920771,297.209925872298));
#8689=CARTESIAN_POINT('Ctrl Pts',(2.10052350874328,-3.32730824867743,297.203777862236));
#8690=CARTESIAN_POINT('Ctrl Pts',(1.99609032587457,-3.38882168473792,297.197629852174));
#8691=CARTESIAN_POINT('Ctrl Pts',(1.89165714300586,-3.45033512079841,297.191481842113));
#8692=CARTESIAN_POINT('Ctrl Pts',(1.78451577278856,-3.50693550549097,297.185333832051));
#8693=CARTESIAN_POINT('Ctrl Pts',(1.67517794669337,-3.5584080495233,297.179185821989));
#8694=CARTESIAN_POINT('Ctrl Pts',(1.57185472735803,-3.60704912047498,297.17337601019));
#8695=CARTESIAN_POINT('Ctrl Pts',(1.46622640852283,-3.65127306702064,297.167566198392));
#8696=CARTESIAN_POINT('Ctrl Pts',(1.35871188831538,-3.69085234120121,297.161756386593));
#8697=CARTESIAN_POINT('Ctrl Pts',(1.25133220858134,-3.73038197661617,297.155953861231));
#8698=CARTESIAN_POINT('Ctrl Pts',(1.14207142311045,-3.76527837434843,297.15015133587));
#8699=CARTESIAN_POINT('Ctrl Pts',(1.03137166586317,-3.79536052132793,297.144348810508));
#8700=CARTESIAN_POINT('Ctrl Pts',(0.916627242200359,-3.82654178769685,297.138334276737));
#8701=CARTESIAN_POINT('Ctrl Pts',(0.80033708804374,-3.85255006284705,297.132319742966));
#8702=CARTESIAN_POINT('Ctrl Pts',(0.683015242738371,-3.87323884858487,297.126305209194));
#8703=CARTESIAN_POINT('Ctrl Pts',(0.570016091063465,-3.89316536126009,297.120512279394));
#8704=CARTESIAN_POINT('Ctrl Pts',(0.456060386669762,-3.90815736014175,297.114719349594));
#8705=CARTESIAN_POINT('Ctrl Pts',(0.341620584758718,-3.9181353187542,297.108926419794));
#8706=CARTESIAN_POINT('Ctrl Pts',(0.227217569652898,-3.92811006994045,297.103135352138));
#8707=CARTESIAN_POINT('Ctrl Pts',(0.112331187183536,-3.9330739474982,297.097344284482));
#8708=CARTESIAN_POINT('Ctrl Pts',(-0.00255992000503504,-3.93299916689663,
297.091553216826));
#8709=CARTESIAN_POINT('Ctrl Pts',(-0.117443336562963,-3.93292439130075,
297.085762536815));
#8710=CARTESIAN_POINT('Ctrl Pts',(-0.232331054333504,-3.92781162915625,
297.079971856804));
#8711=CARTESIAN_POINT('Ctrl Pts',(-0.346744203551527,-3.91768521671961,
297.074181176793));
#8712=CARTESIAN_POINT('Ctrl Pts',(-0.461178814918284,-3.9075569047236,297.068389410539));
#8713=CARTESIAN_POINT('Ctrl Pts',(-0.575138259774275,-3.89241311188772,
297.062597644286));
#8714=CARTESIAN_POINT('Ctrl Pts',(-0.688149404645904,-3.872329970042,297.056805878032));
#8715=CARTESIAN_POINT('Ctrl Pts',(-0.801268442345112,-3.8522276546275,297.051008582323));
#8716=CARTESIAN_POINT('Ctrl Pts',(-0.913436956617779,-3.82717665357635,
297.045211286614));
#8717=CARTESIAN_POINT('Ctrl Pts',(-1.02419272669782,-3.7973040777082,297.039413990906));
#8718=CARTESIAN_POINT('Ctrl Pts',(-1.1350116354853,-3.76741447233605,297.033613390324));
#8719=CARTESIAN_POINT('Ctrl Pts',(-1.24441579482542,-3.73269794898566,297.027812789742));
#8720=CARTESIAN_POINT('Ctrl Pts',(-1.35196052638055,-3.6933307102274,297.022012189161));
#8721=CARTESIAN_POINT('Ctrl Pts',(-1.45965001674123,-3.65391048184912,297.016203780776));
#8722=CARTESIAN_POINT('Ctrl Pts',(-1.56547469669027,-3.60982721005101,297.010395372392));
#8723=CARTESIAN_POINT('Ctrl Pts',(-1.6690122428726,-3.56130413376075,297.004586964008));
#8724=CARTESIAN_POINT('Ctrl Pts',(-1.6962671560051,-3.54853106468604,297.003057976006));
#8725=CARTESIAN_POINT('Ctrl Pts',(-1.72336373148895,-3.53545058421414,297.001528988003));
#8726=CARTESIAN_POINT('Ctrl Pts',(-1.75029459251059,-3.52206726787383,297.));
#8727=CARTESIAN_POINT('Ctrl Pts',(-1.75029459251059,-3.52206726787383,297.));
#8728=CARTESIAN_POINT('Ctrl Pts',(-1.77179842669062,-3.5111330638087,297.));
#8729=CARTESIAN_POINT('Ctrl Pts',(-1.79330226087066,-3.50019885974357,297.));
#8730=CARTESIAN_POINT('Ctrl Pts',(-1.8148060950507,-3.48926465567845,297.));
#8731=CARTESIAN_POINT('Origin',(0.,0.,294.689226550727));
#8732=CARTESIAN_POINT('',(-1.83773660687461,2.64742171296018,307.));
#8733=CARTESIAN_POINT('Ctrl Pts',(-1.83773660687461,2.64742171296018,307.));
#8734=CARTESIAN_POINT('Ctrl Pts',(-1.61287070412985,2.80351482766456,306.981925201061));
#8735=CARTESIAN_POINT('Ctrl Pts',(-1.36896672511014,2.93037193689488,306.963084112479));
#8736=CARTESIAN_POINT('Ctrl Pts',(-1.05017572288253,3.04755119987033,306.940809548134));
#8737=CARTESIAN_POINT('Ctrl Pts',(-0.987803804135199,3.06833536507446,306.936547798351));
#8738=CARTESIAN_POINT('Ctrl Pts',(-0.871840468484198,3.1030746666412,306.928803430231));
#8739=CARTESIAN_POINT('Ctrl Pts',(-0.818442098850674,3.11758421031641,306.925305496342));
#8740=CARTESIAN_POINT('Ctrl Pts',(-0.728882018453243,3.13945975844889,306.919548036367));
#8741=CARTESIAN_POINT('Ctrl Pts',(-0.692921543180439,3.1475921720448,306.917265149125));
#8742=CARTESIAN_POINT('Ctrl Pts',(-0.620633318897018,3.1626410950454,306.912730943104));
#8743=CARTESIAN_POINT('Ctrl Pts',(-0.584310338013351,3.16955296720124,306.910480077154));
#8744=CARTESIAN_POINT('Ctrl Pts',(-0.492739779393588,3.18535013274941,306.9048694953));
#8745=CARTESIAN_POINT('Ctrl Pts',(-0.437363761211979,3.19342471899757,306.901534730072));
#8746=CARTESIAN_POINT('Ctrl Pts',(-0.164547752393253,3.22597479512708,306.885344468204));
#8747=CARTESIAN_POINT('Ctrl Pts',(0.0547837142037089,3.22970538388019,306.873117270049));
#8748=CARTESIAN_POINT('Ctrl Pts',(0.380689913146888,3.20201715200492,306.854682802465));
#8749=CARTESIAN_POINT('Ctrl Pts',(0.488029488352053,3.1874226923407,306.848557386198));
#8750=CARTESIAN_POINT('Ctrl Pts',(0.638836058752621,3.15912137709952,306.839643332122));
#8751=CARTESIAN_POINT('Ctrl Pts',(0.683065213441602,3.14985411486993,306.836990481927));
#8752=CARTESIAN_POINT('Ctrl Pts',(0.761855729305654,3.13160779863767,306.832172485715));
#8753=CARTESIAN_POINT('Ctrl Pts',(0.796490807200217,3.12297834146815,306.830022269894));
#8754=CARTESIAN_POINT('Ctrl Pts',(0.851768223127815,3.10822644914928,306.826528210933));
#8755=CARTESIAN_POINT('Ctrl Pts',(0.872505836561738,3.10246906040753,306.825203193745));
#8756=CARTESIAN_POINT('Ctrl Pts',(0.91403557023949,3.09048985150914,306.82251821819));
#8757=CARTESIAN_POINT('Ctrl Pts',(0.934825550593697,3.08426485055132,306.821158100424));
#8758=CARTESIAN_POINT('Ctrl Pts',(0.990984156166277,3.06682972145306,306.817443537762));
#8759=CARTESIAN_POINT('Ctrl Pts',(1.02622371080723,3.05521828511104,306.815068765204));
#8760=CARTESIAN_POINT('Ctrl Pts',(1.23466757292442,2.98252305104199,306.800790453124));
#8761=CARTESIAN_POINT('Ctrl Pts',(1.40258282254529,2.90733561485834,306.788350032493));
#8762=CARTESIAN_POINT('Ctrl Pts',(1.73915739230668,2.72065238146191,306.762428562735));
#8763=CARTESIAN_POINT('Ctrl Pts',(1.90563882353315,2.60675666300069,306.749030436459));
#8764=CARTESIAN_POINT('Ctrl Pts',(2.10080242353114,2.44448445893484,306.732834129059));
#8765=CARTESIAN_POINT('Ctrl Pts',(2.14035554269547,2.40992816212038,306.729520558536));
#8766=CARTESIAN_POINT('Ctrl Pts',(2.20580482506759,2.34986414217837,306.723980701444));
#8767=CARTESIAN_POINT('Ctrl Pts',(2.23214511916507,2.32485800576727,306.721734693006));
#8768=CARTESIAN_POINT('Ctrl Pts',(2.28162669112034,2.27626632300347,306.717481060624));
#8769=CARTESIAN_POINT('Ctrl Pts',(2.30483879201089,2.2527598619761,306.715470504151));
#8770=CARTESIAN_POINT('Ctrl Pts',(2.36549664247051,2.18941362276678,306.710172082117));
#8771=CARTESIAN_POINT('Ctrl Pts',(2.40229783085265,2.14896998990693,306.706911093949));
#8772=CARTESIAN_POINT('Ctrl Pts',(2.59380992471914,1.92743124043834,306.689640868596));
#8773=CARTESIAN_POINT('Ctrl Pts',(2.72911359781551,1.73054601380094,306.676412443957));
#8774=CARTESIAN_POINT('Ctrl Pts',(2.88999641078797,1.42989734306044,306.65721659348));
#8775=CARTESIAN_POINT('Ctrl Pts',(2.93413220223388,1.33699348973775,306.651396244909));
#8776=CARTESIAN_POINT('Ctrl Pts',(2.99067309033731,1.20163210406146,306.642870217234));
#8777=CARTESIAN_POINT('Ctrl Pts',(3.00676516545293,1.16077911378317,306.640291048985));
#8778=CARTESIAN_POINT('Ctrl Pts',(3.03414481857618,1.0868769260064,306.635593691662));
#8779=CARTESIAN_POINT('Ctrl Pts',(3.04573944202751,1.05394841661457,306.633489605921));
#8780=CARTESIAN_POINT('Ctrl Pts',(3.06351637601019,1.00071726389996,306.630060821614));
#8781=CARTESIAN_POINT('Ctrl Pts',(3.07003729912584,0.98052973061205,306.628754220295));
#8782=CARTESIAN_POINT('Ctrl Pts',(3.08276120522064,0.939767353358554,306.626100664425));
#8783=CARTESIAN_POINT('Ctrl Pts',(3.08895863951121,0.919191921180365,306.624753465552));
#8784=CARTESIAN_POINT('Ctrl Pts',(3.10519172891196,0.863279377217664,306.621074413987));
#8785=CARTESIAN_POINT('Ctrl Pts',(3.11482942403955,0.827831116045951,306.618722444911));
#8786=CARTESIAN_POINT('Ctrl Pts',(3.17032298187014,0.609012655509117,306.60411652629));
#8787=CARTESIAN_POINT('Ctrl Pts',(3.20057583201716,0.422077655409949,306.591287083847));
#8788=CARTESIAN_POINT('Ctrl Pts',(3.22389613507508,0.101173973082913,306.569606783471));
#8789=CARTESIAN_POINT('Ctrl Pts',(3.22532816999698,-0.0317127598530274,
306.560722540597));
#8790=CARTESIAN_POINT('Ctrl Pts',(3.21538154062596,-0.226541299232325,306.547960786327));
#8791=CARTESIAN_POINT('Ctrl Pts',(3.21040093963496,-0.288662434806583,306.543929938373));
#8792=CARTESIAN_POINT('Ctrl Pts',(3.19785373624608,-0.403311926627462,306.536564443814));
#8793=CARTESIAN_POINT('Ctrl Pts',(3.19078516043562,-0.455872363121254,306.533216631283));
#8794=CARTESIAN_POINT('Ctrl Pts',(3.1767224450102,-0.543928727000493,306.527653573156));
#8795=CARTESIAN_POINT('Ctrl Pts',(3.17042222253808,-0.579523122859388,306.525417464515));
#8796=CARTESIAN_POINT('Ctrl Pts',(3.15649363764549,-0.65117035338417,306.520939473213));
#8797=CARTESIAN_POINT('Ctrl Pts',(3.14884309553138,-0.687213390501681,306.518698648962));
#8798=CARTESIAN_POINT('Ctrl Pts',(3.1278179843444,-0.778527551955302,306.513047107254));
#8799=CARTESIAN_POINT('Ctrl Pts',(3.11359538902554,-0.833591517412508,306.509663286526));
#8800=CARTESIAN_POINT('Ctrl Pts',(3.03787008771021,-1.09769549607522,306.493504476644));
#8801=CARTESIAN_POINT('Ctrl Pts',(2.95673330280883,-1.30051054264951,306.481360031334));
#8802=CARTESIAN_POINT('Ctrl Pts',(2.7789395820027,-1.64045011348556,306.459829428575));
#8803=CARTESIAN_POINT('Ctrl Pts',(2.69092958273882,-1.78114222663982,306.450494482124));
#8804=CARTESIAN_POINT('Ctrl Pts',(2.57258227108704,-1.94140745585752,306.43860712754));
#8805=CARTESIAN_POINT('Ctrl Pts',(2.55223961579672,-1.96807398148679,306.43658376302));
#8806=CARTESIAN_POINT('Ctrl Pts',(2.51860192680313,-2.0107698268558,306.433260970514));
#8807=CARTESIAN_POINT('Ctrl Pts',(2.50556052904555,-2.026997131263,306.431978046634));
#8808=CARTESIAN_POINT('Ctrl Pts',(2.47854663321916,-2.0599512410396,306.429328855182));
#8809=CARTESIAN_POINT('Ctrl Pts',(2.46456011484081,-2.07666461090596,306.427961788277));
#8810=CARTESIAN_POINT('Ctrl Pts',(2.42571484417746,-2.12213810179588,306.424180373945));
#8811=CARTESIAN_POINT('Ctrl Pts',(2.40051576363387,-2.1506014074319,306.421744235517));
#8812=CARTESIAN_POINT('Ctrl Pts',(2.26342559396227,-2.30003815802544,306.408609366423));
#8813=CARTESIAN_POINT('Ctrl Pts',(2.14288977364294,-2.41273426330881,306.397482752757));
#8814=CARTESIAN_POINT('Ctrl Pts',(1.89959055234895,-2.60753877182522,306.376464665738));
#8815=CARTESIAN_POINT('Ctrl Pts',(1.77875099969262,-2.69142224501287,306.366593040309));
#8816=CARTESIAN_POINT('Ctrl Pts',(1.59613125004096,-2.80050159449724,306.352642675542));
#8817=CARTESIAN_POINT('Ctrl Pts',(1.53863893246068,-2.83249629952332,306.348377331761));
#8818=CARTESIAN_POINT('Ctrl Pts',(1.43113267567081,-2.88808391054059,306.340634354899));
#8819=CARTESIAN_POINT('Ctrl Pts',(1.38141437204418,-2.91219235790896,306.337141198978));
#8820=CARTESIAN_POINT('Ctrl Pts',(1.29768657491515,-2.95016492355461,306.33139954886));
#8821=CARTESIAN_POINT('Ctrl Pts',(1.26401748154344,-2.96474678555149,306.329127536149));
#8822=CARTESIAN_POINT('Ctrl Pts',(1.19620664627505,-2.99274996149709,306.32462220454));
#8823=CARTESIAN_POINT('Ctrl Pts',(1.16207017945549,-3.00616961239103,306.322389208966));
#8824=CARTESIAN_POINT('Ctrl Pts',(1.07601618947093,-3.03831399744688,306.316842589215));
#8825=CARTESIAN_POINT('Ctrl Pts',(1.02383193274198,-3.05629374959402,306.313553256359));
#8826=CARTESIAN_POINT('Ctrl Pts',(0.720205987844388,-3.15225584394364,306.29478903629));
#8827=CARTESIAN_POINT('Ctrl Pts',(0.460437782574308,-3.20053370881745,306.280298475396));
#8828=CARTESIAN_POINT('Ctrl Pts',(0.112490426482024,-3.22191689234664,306.260584485301));
#8829=CARTESIAN_POINT('Ctrl Pts',(0.0271290448312729,-3.22376565431938,
306.255714483836));
#8830=CARTESIAN_POINT('Ctrl Pts',(-0.113940200882418,-3.22121765483144,
306.247474244329));
#8831=CARTESIAN_POINT('Ctrl Pts',(-0.169641527447385,-3.21876475248769,
306.24417080106));
#8832=CARTESIAN_POINT('Ctrl Pts',(-0.250279827510826,-3.21311488396034,
306.23928090679));
#8833=CARTESIAN_POINT('Ctrl Pts',(-0.275289797258755,-3.21106877645816,
306.237749244342));
#8834=CARTESIAN_POINT('Ctrl Pts',(-0.32011990641438,-3.20687358346846,306.234972670186));
#8835=CARTESIAN_POINT('Ctrl Pts',(-0.339948087770548,-3.20483231558631,
306.233733381659));
#8836=CARTESIAN_POINT('Ctrl Pts',(-0.385993150355525,-3.19965996883413,
306.230829534818));
#8837=CARTESIAN_POINT('Ctrl Pts',(-0.412191956711931,-3.1963905134471,306.229158052042));
#8838=CARTESIAN_POINT('Ctrl Pts',(-0.497754600274649,-3.18464342612453,
306.223642456298));
#8839=CARTESIAN_POINT('Ctrl Pts',(-0.556919617412703,-3.17483117603528,
306.219739095561));
#8840=CARTESIAN_POINT('Ctrl Pts',(-0.814290122059809,-3.12473226156958,
306.202460057997));
#8841=CARTESIAN_POINT('Ctrl Pts',(-1.00872586434939,-3.06748952045082,306.188656788649));
#8842=CARTESIAN_POINT('Ctrl Pts',(-1.2911322661333,-2.95456919024241,306.168317470085));
#8843=CARTESIAN_POINT('Ctrl Pts',(-1.3839091307744,-2.91226714546435,306.161577908947));
#8844=CARTESIAN_POINT('Ctrl Pts',(-1.47484249366466,-2.86547680213046,306.154940145955));
#8845=CARTESIAN_POINT('Ctrl Pts',(-1.47515326121876,-2.86531683075061,306.154917460778));
#8846=CARTESIAN_POINT('Ctrl Pts',(-1.47546400238914,-2.86515680899909,306.154894777109));
#8847=CARTESIAN_POINT('',(1.87158653173908,2.62360084935054,307.));
#8848=CARTESIAN_POINT('Origin',(0.,0.,307.));
#8849=CARTESIAN_POINT('',(3.22274974449961,-0.00128328785181631,306.810773449319));
#8850=CARTESIAN_POINT('Ctrl Pts',(3.22274974449961,-0.00128328785181409,
306.810773449319));
#8851=CARTESIAN_POINT('Ctrl Pts',(3.2227900185038,0.0998577278200301,306.817062136975));
#8852=CARTESIAN_POINT('Ctrl Pts',(3.21806481467562,0.201159732219282,306.823350824632));
#8853=CARTESIAN_POINT('Ctrl Pts',(3.20855495035338,0.302146807136616,306.829639512289));
#8854=CARTESIAN_POINT('Ctrl Pts',(3.19905935199351,0.402982389060622,306.835918766144));
#8855=CARTESIAN_POINT('Ctrl Pts',(3.1847934102067,0.503503571635619,306.842198019998));
#8856=CARTESIAN_POINT('Ctrl Pts',(3.16578993983136,0.603234298894355,306.848477273852));
#8857=CARTESIAN_POINT('Ctrl Pts',(3.1466829878995,0.703508100164581,306.854790720775));
#8858=CARTESIAN_POINT('Ctrl Pts',(3.12278673719962,0.802982385591739,306.861104167698));
#8859=CARTESIAN_POINT('Ctrl Pts',(3.09418761530848,0.901177320937233,306.867417614621));
#8860=CARTESIAN_POINT('Ctrl Pts',(3.06581086092608,0.998608758605197,306.873681972433));
#8861=CARTESIAN_POINT('Ctrl Pts',(3.03280421803192,1.09478026340372,306.879946330245));
#8862=CARTESIAN_POINT('Ctrl Pts',(2.9953032935351,1.18923325812803,306.886210688057));
#8863=CARTESIAN_POINT('Ctrl Pts',(2.95782620525254,1.28362621695055,306.892471064138));
#8864=CARTESIAN_POINT('Ctrl Pts',(2.91586067103949,1.37630245420618,306.89873144022));
#8865=CARTESIAN_POINT('Ctrl Pts',(2.86959151116524,1.46682041216653,306.904991816301));
#8866=CARTESIAN_POINT('Ctrl Pts',(2.82334098226624,1.55730192170554,306.911249671548));
#8867=CARTESIAN_POINT('Ctrl Pts',(2.77279046509754,1.64562651266173,306.917507526795));
#8868=CARTESIAN_POINT('Ctrl Pts',(2.71817178259418,1.73137509593062,306.923765382041));
#8869=CARTESIAN_POINT('Ctrl Pts',(2.66272368003668,1.81842582695039,306.930118266871));
#8870=CARTESIAN_POINT('Ctrl Pts',(2.60308303061169,1.90282127450765,306.936471151701));
#8871=CARTESIAN_POINT('Ctrl Pts',(2.53953908698161,1.98415190653151,306.942824036531));
#8872=CARTESIAN_POINT('Ctrl Pts',(2.47693440670235,2.06428036447558,306.949083017339));
#8873=CARTESIAN_POINT('Ctrl Pts',(2.41054134049455,2.14143369306294,306.955341998146));
#8874=CARTESIAN_POINT('Ctrl Pts',(2.34067753745869,2.21525308444347,306.961600978954));
#8875=CARTESIAN_POINT('Ctrl Pts',(2.26924147554104,2.2907337537491,306.968000815795));
#8876=CARTESIAN_POINT('Ctrl Pts',(2.19417688390513,2.36272828260635,306.974400652636));
#8877=CARTESIAN_POINT('Ctrl Pts',(2.11586276660478,2.43089331633364,306.980800489477));
#8878=CARTESIAN_POINT('Ctrl Pts',(2.03754864930444,2.49905835006092,306.987200326318));
#8879=CARTESIAN_POINT('Ctrl Pts',(1.95598538003388,2.56339361630214,306.993600163159));
#8880=CARTESIAN_POINT('Ctrl Pts',(1.87158653173908,2.62360084935054,307.));
#8881=CARTESIAN_POINT('Ctrl Pts',(-1.47546400239267,-2.86515680899727,306.403639991207));
#8882=CARTESIAN_POINT('Ctrl Pts',(-1.44148025683963,-2.88265734965617,306.406010377244));
#8883=CARTESIAN_POINT('Ctrl Pts',(-1.4072048219913,-2.89954303224035,306.408380763282));
#8884=CARTESIAN_POINT('Ctrl Pts',(-1.37266201798484,-2.91580461397567,306.410751149319));
#8885=CARTESIAN_POINT('Ctrl Pts',(-1.28260809080463,-2.95819895165459,306.416930803164));
#8886=CARTESIAN_POINT('Ctrl Pts',(-1.19043722760257,-2.99648857823904,306.42311045701));
#8887=CARTESIAN_POINT('Ctrl Pts',(-1.09655907514793,-3.03045801112814,306.429290110855));
#8888=CARTESIAN_POINT('Ctrl Pts',(-1.00280319052376,-3.06438320189324,306.435461716258));
#8889=CARTESIAN_POINT('Ctrl Pts',(-0.907344840639183,-3.09399923764599,
306.441633321662));
#8890=CARTESIAN_POINT('Ctrl Pts',(-0.810616121734273,-3.11913755158128,
306.447804927065));
#8891=CARTESIAN_POINT('Ctrl Pts',(-0.713985031579461,-3.14425049329831,
306.453970303438));
#8892=CARTESIAN_POINT('Ctrl Pts',(-0.616086538789796,-3.16489459080302,
306.460135679811));
#8893=CARTESIAN_POINT('Ctrl Pts',(-0.517369577501691,-3.18095053133112,
306.466301056184));
#8894=CARTESIAN_POINT('Ctrl Pts',(-0.41871866805352,-3.19699572877718,306.472462307283));
#8895=CARTESIAN_POINT('Ctrl Pts',(-0.31925080513799,-3.20845880339074,306.478623558383));
#8896=CARTESIAN_POINT('Ctrl Pts',(-0.219425976298026,-3.21527134211495,
306.484784809483));
#8897=CARTESIAN_POINT('Ctrl Pts',(-0.119634950830539,-3.22208157393028,
306.490943974217));
#8898=CARTESIAN_POINT('Ctrl Pts',(-0.0194876312642712,-3.22424436990655,
306.497103138951));
#8899=CARTESIAN_POINT('Ctrl Pts',(0.0805508922861619,-3.22174317974787,
306.503262303685));
#8900=CARTESIAN_POINT('Ctrl Pts',(0.180582091152676,-3.21924217272291,306.509421017454));
#8901=CARTESIAN_POINT('Ctrl Pts',(0.280504076959468,-3.21207786961416,306.515579731223));
#8902=CARTESIAN_POINT('Ctrl Pts',(0.379852771505078,-3.20028583637148,306.521738444991));
#8903=CARTESIAN_POINT('Ctrl Pts',(0.479220559436792,-3.1884915368701,306.527898342376));
#8904=CARTESIAN_POINT('Ctrl Pts',(0.5780144072396,-3.17206779140419,306.53405823976));
#8905=CARTESIAN_POINT('Ctrl Pts',(0.675777349248666,-3.1511017972675,306.540218137145));
#8906=CARTESIAN_POINT('Ctrl Pts',(0.773645906311291,-3.13011315319261,306.546384689177));
#8907=CARTESIAN_POINT('Ctrl Pts',(0.870480909905088,-3.10457255410761,306.552551241208));
#8908=CARTESIAN_POINT('Ctrl Pts',(0.965837679616123,-3.07461788506047,306.55871779324));
#8909=CARTESIAN_POINT('Ctrl Pts',(1.06125042793634,-3.04464563130785,306.564887965309));
#8910=CARTESIAN_POINT('Ctrl Pts',(1.1551828078156,-3.01025429615689,306.571058137377));
#8911=CARTESIAN_POINT('Ctrl Pts',(1.24720927533731,-2.97163029093671,306.577228309446));
#8912=CARTESIAN_POINT('Ctrl Pts',(1.3393842130672,-2.93294397196864,306.583408436115));
#8913=CARTESIAN_POINT('Ctrl Pts',(1.42964670704646,-2.89001153183243,306.589588562784));
#8914=CARTESIAN_POINT('Ctrl Pts',(1.51759496417796,-2.84306579016415,306.595768689453));
#8915=CARTESIAN_POINT('Ctrl Pts',(1.57166611144707,-2.81420324991383,306.599568270595));
#8916=CARTESIAN_POINT('Ctrl Pts',(1.62486303875039,-2.78382461569644,306.603367851737));
#8917=CARTESIAN_POINT('Ctrl Pts',(1.67709810690495,-2.75199191537981,306.607167432879));
#8918=CARTESIAN_POINT('Ctrl Pts',(1.76153937550061,-2.7005323558822,306.61330969445));
#8919=CARTESIAN_POINT('Ctrl Pts',(1.84376394271427,-2.64508882172917,306.61945195602));
#8920=CARTESIAN_POINT('Ctrl Pts',(1.92336899553465,-2.58587881957296,306.625594217591));
#8921=CARTESIAN_POINT('Ctrl Pts',(2.00286782485598,-2.52674782614025,306.631728283042));
#8922=CARTESIAN_POINT('Ctrl Pts',(2.0797537364873,-2.46386061159534,306.637862348493));
#8923=CARTESIAN_POINT('Ctrl Pts',(2.15365030406937,-2.39747949527872,306.643996413945));
#8924=CARTESIAN_POINT('Ctrl Pts',(2.22747066260521,-2.33116683737266,306.650124153374));
#8925=CARTESIAN_POINT('Ctrl Pts',(2.29830747988894,-2.26136773151431,306.656251892804));
#8926=CARTESIAN_POINT('Ctrl Pts',(2.36581585552691,-2.1883859120908,306.662379632234));
#8927=CARTESIAN_POINT('Ctrl Pts',(2.43327891022544,-2.11545308813765,306.668503257879));
#8928=CARTESIAN_POINT('Ctrl Pts',(2.49741766648453,-2.03934211823852,306.674626883524));
#8929=CARTESIAN_POINT('Ctrl Pts',(2.55792339060626,-1.96039421808201,306.680750509169));
#8930=CARTESIAN_POINT('Ctrl Pts',(2.61840867311654,-1.8814729901507,306.686872065973));
#8931=CARTESIAN_POINT('Ctrl Pts',(2.675263094699,-1.79971708409036,306.692993622776));
#8932=CARTESIAN_POINT('Ctrl Pts',(2.72821825743358,-1.71550071474951,306.69911517958));
#8933=CARTESIAN_POINT('Ctrl Pts',(2.781170055598,-1.6312896961973,306.705236347442));
#8934=CARTESIAN_POINT('Ctrl Pts',(2.83022285364238,-1.54461889699493,306.711357515305));
#8935=CARTESIAN_POINT('Ctrl Pts',(2.87515223598542,-1.45589051182018,306.717478683168));
#8936=CARTESIAN_POINT('Ctrl Pts',(2.92009108854134,-1.36714342448101,306.72360114125));
#8937=CARTESIAN_POINT('Ctrl Pts',(2.96090460081192,-1.2763382816299,306.729723599333));
#8938=CARTESIAN_POINT('Ctrl Pts',(2.99741534562876,-1.18389983034429,306.735846057415));
#8939=CARTESIAN_POINT('Ctrl Pts',(3.03396812778423,-1.09135494829429,306.741975564705));
#8940=CARTESIAN_POINT('Ctrl Pts',(3.06620809057851,-0.997173412699476,306.748105071996));
#8941=CARTESIAN_POINT('Ctrl Pts',(3.09400687590812,-0.901797657090131,306.754234579286));
#8942=CARTESIAN_POINT('Ctrl Pts',(3.12182281687966,-0.806363041631609,306.760367869319));
#8943=CARTESIAN_POINT('Ctrl Pts',(3.14519202204811,-0.709733165797646,306.766501159351));
#8944=CARTESIAN_POINT('Ctrl Pts',(3.16403720627626,-0.612361102454695,306.772634449384));
#8945=CARTESIAN_POINT('Ctrl Pts',(3.18291493122178,-0.514820902957957,306.778778330008));
#8946=CARTESIAN_POINT('Ctrl Pts',(3.197252973546,-0.416536391159208,306.784922210633));
#8947=CARTESIAN_POINT('Ctrl Pts',(3.20702588338914,-0.317966265147866,306.791066091258));
#8948=CARTESIAN_POINT('Ctrl Pts',(3.21366303612879,-0.2510235641096,306.795238632985));
#8949=CARTESIAN_POINT('Ctrl Pts',(3.21819571122489,-0.183949193495648,306.799411174712));
#8950=CARTESIAN_POINT('Ctrl Pts',(3.2206296272874,-0.116886125517962,306.80358371644));
#8951=CARTESIAN_POINT('Ctrl Pts',(3.22202759263413,-0.0783671944331345,
306.805980294051));
#8952=CARTESIAN_POINT('Ctrl Pts',(3.22273439633175,-0.0398274661541265,
306.808376871662));
#8953=CARTESIAN_POINT('Ctrl Pts',(3.22274974449932,-0.00128328858516614,
306.810773449273));
#8954=CARTESIAN_POINT('Ctrl Pts',(1.43037091239959,-2.88157788358434,296.586649784659));
#8955=CARTESIAN_POINT('Ctrl Pts',(2.37869428028674,-2.41084475896467,296.652121879179));
#8956=CARTESIAN_POINT('Ctrl Pts',(3.75821890350017,-0.46632426907627,296.783066068219));
#8957=CARTESIAN_POINT('Ctrl Pts',(2.46052379546342,2.88456422682259,296.97948235178));
#8958=CARTESIAN_POINT('Ctrl Pts',(-1.05164585738147,3.64025694602008,297.17589863534));
#8959=CARTESIAN_POINT('Ctrl Pts',(-3.61728260103292,1.12907581019222,297.3723149189));
#8960=CARTESIAN_POINT('Ctrl Pts',(-2.93521143642197,-2.39722873440577,297.56873120246));
#8961=CARTESIAN_POINT('Ctrl Pts',(0.383440535871874,-3.77005108800603,297.765147486021));
#8962=CARTESIAN_POINT('Ctrl Pts',(3.35750728960981,-1.75722429176289,297.96156376958));
#8963=CARTESIAN_POINT('Ctrl Pts',(3.3162883264954,1.8338860675821,298.157980053141));
#8964=CARTESIAN_POINT('Ctrl Pts',(0.296653368432913,3.77792383424779,298.354396336701));
#8965=CARTESIAN_POINT('Ctrl Pts',(-2.98938444913632,2.32902251834708,298.550812620261));
#8966=CARTESIAN_POINT('Ctrl Pts',(-3.59065782085272,-1.21159272548526,298.747228903822));
#8967=CARTESIAN_POINT('Ctrl Pts',(-0.96714588876518,-3.66406736193667,298.943645187382));
#8968=CARTESIAN_POINT('Ctrl Pts',(2.5249602887996,-2.82583495365449,299.140061470942));
#8969=CARTESIAN_POINT('Ctrl Pts',(3.74939329087914,0.550289383578493,299.336477754502));
#8970=CARTESIAN_POINT('Ctrl Pts',(1.6064846293266,3.43219662332693,299.532894038062));
#8971=CARTESIAN_POINT('Ctrl Pts',(-1.97921236533452,3.23163824688042,299.729310321623));
#8972=CARTESIAN_POINT('Ctrl Pts',(-3.78737302228878,0.128735920266949,299.925726605183));
#8973=CARTESIAN_POINT('Ctrl Pts',(-2.19408276686631,-3.08978445485654,300.122142888743));
#8974=CARTESIAN_POINT('Ctrl Pts',(1.36971965459014,-3.53336034491094,300.318559172303));
#8975=CARTESIAN_POINT('Ctrl Pts',(3.70337283434201,-0.803614895688885,300.514975455864));
#8976=CARTESIAN_POINT('Ctrl Pts',(2.71101596545655,2.64785945046433,300.711391739424));
#8977=CARTESIAN_POINT('Ctrl Pts',(-0.716112319080844,3.72128343332825,300.907808022984));
#8978=CARTESIAN_POINT('Ctrl Pts',(-3.50009802324731,1.45261181002151,301.104224306544));
#8979=CARTESIAN_POINT('Ctrl Pts',(-3.14063538989392,-2.12065475486385,301.300640590105));
#8980=CARTESIAN_POINT('Ctrl Pts',(0.0394411310795686,-3.78935504273392,
301.497056873665));
#8981=CARTESIAN_POINT('Ctrl Pts',(3.18409545625435,-2.05482441288724,301.693473157225));
#8982=CARTESIAN_POINT('Ctrl Pts',(3.46910427998845,1.5251500702891,301.889889440785));
#8983=CARTESIAN_POINT('Ctrl Pts',(0.638500338801349,3.73538278628368,302.086305724345));
#8984=CARTESIAN_POINT('Ctrl Pts',(-2.76554263595121,2.5908572269264,302.282722007906));
#8985=CARTESIAN_POINT('Ctrl Pts',(-3.68584362940364,-0.880524833572776,
302.479138291466));
#8986=CARTESIAN_POINT('Ctrl Pts',(-1.29587760982979,-3.56110495001826,302.675554575026));
#8987=CARTESIAN_POINT('Ctrl Pts',(2.25791990446593,-3.04344622745171,302.871970858586));
#8988=CARTESIAN_POINT('Ctrl Pts',(3.78387290864046,0.207540506822766,303.068387142146));
#8989=CARTESIAN_POINT('Ctrl Pts',(1.91151851156535,3.2721345081006,303.264803425707));
#8990=CARTESIAN_POINT('Ctrl Pts',(-1.67757627766529,3.39801486134882,303.461219709267));
#8991=CARTESIAN_POINT('Ctrl Pts',(-3.76003489430519,0.472128097803197,303.657635992827));
#8992=CARTESIAN_POINT('Ctrl Pts',(-2.46559506200593,-2.87777836811756,303.854052276388));
#8993=CARTESIAN_POINT('Ctrl Pts',(1.04320286127918,-3.643143466247,304.050468559947));
#8994=CARTESIAN_POINT('Ctrl Pts',(3.61509741898655,-1.13659100234235,304.246884843508));
#8995=CARTESIAN_POINT('Ctrl Pts',(2.94026192950194,2.39073784243107,304.443301127068));
#8996=CARTESIAN_POINT('Ctrl Pts',(-0.375230571251665,3.77093659736716,304.639717410628));
#8997=CARTESIAN_POINT('Ctrl Pts',(-3.35372926879606,1.7644490671369,304.836133694189));
#8998=CARTESIAN_POINT('Ctrl Pts',(-3.32022984313726,-1.82670169005412,305.032549977749));
#8999=CARTESIAN_POINT('Ctrl Pts',(-0.304830726285696,-3.77727281867384,
305.228966261309));
#9000=CARTESIAN_POINT('Ctrl Pts',(2.98435586070458,-2.33549276813259,305.425382544869));
#9001=CARTESIAN_POINT('Ctrl Pts',(3.59324514050816,1.20386119281218,305.621798828429));
#9002=CARTESIAN_POINT('Ctrl Pts',(0.975112331956289,3.66189401687049,305.81821511199));
#9003=CARTESIAN_POINT('Ctrl Pts',(-2.51894641698954,2.83144498973554,306.01463139555));
#9004=CARTESIAN_POINT('Ctrl Pts',(-3.75036188556599,-0.542523113047413,
306.21104767911));
#9005=CARTESIAN_POINT('Ctrl Pts',(-1.61436456647499,-3.42801060221597,306.40746396267));
#9006=CARTESIAN_POINT('Ctrl Pts',(1.97313131176253,-3.23753624740303,306.60388024623));
#9007=CARTESIAN_POINT('Ctrl Pts',(3.78506371541952,-0.133490475520108,306.800340127458));
#9008=CARTESIAN_POINT('Ctrl Pts',(2.72947568708186,2.00554125229389,306.931327914165));
#9009=CARTESIAN_POINT('Ctrl Pts',(1.8665577825944,2.62019345361895,306.996843606352));
#9010=CARTESIAN_POINT('Ctrl Pts',(1.53690913862227,-3.0962062668787,296.724992037258));
#9011=CARTESIAN_POINT('Ctrl Pts',(2.55586641595513,-2.5904115567035,296.790464131778));
#9012=CARTESIAN_POINT('Ctrl Pts',(4.03814208444891,-0.501057470123149,296.921408320818));
#9013=CARTESIAN_POINT('Ctrl Pts',(2.64379083373645,3.09941504173152,297.117824604378));
#9014=CARTESIAN_POINT('Ctrl Pts',(-1.12997552927888,3.91139397394884,297.314240887938));
#9015=CARTESIAN_POINT('Ctrl Pts',(-3.88670843227672,1.21317269236876,297.510657171498));
#9016=CARTESIAN_POINT('Ctrl Pts',(-3.15383460424095,-2.57578137064835,297.707073455059));
#9017=CARTESIAN_POINT('Ctrl Pts',(0.412000313059402,-4.05085556480515,297.903489738619));
#9018=CARTESIAN_POINT('Ctrl Pts',(3.60758429275907,-1.88810751757302,298.099906022179));
#9019=CARTESIAN_POINT('Ctrl Pts',(3.56329522022138,1.97047928759305,298.29632230574));
#9020=CARTESIAN_POINT('Ctrl Pts',(0.318748982515844,4.05931469630743,298.4927385893));
#9021=CARTESIAN_POINT('Ctrl Pts',(-3.21204258203581,2.50249495531178,298.68915487286));
#9022=CARTESIAN_POINT('Ctrl Pts',(-3.85810056027791,-1.30183570984583,298.88557115642));
#9023=CARTESIAN_POINT('Ctrl Pts',(-1.03918175484326,-3.93697785956856,299.08198743998));
#9024=CARTESIAN_POINT('Ctrl Pts',(2.71302674633131,-3.03631143982363,299.278403723541));
#9025=CARTESIAN_POINT('Ctrl Pts',(4.0286591142811,0.591276552939527,299.474820007101));
#9026=CARTESIAN_POINT('Ctrl Pts',(1.72614032239109,3.68783670739665,299.671236290661));
#9027=CARTESIAN_POINT('Ctrl Pts',(-2.12662991479166,3.47234015407905,299.867652574221));
#9028=CARTESIAN_POINT('Ctrl Pts',(-4.06946768762379,0.138324549675935,300.064068857781));
#9029=CARTESIAN_POINT('Ctrl Pts',(-2.35750449485402,-3.31992067503358,300.260485141342));
#9030=CARTESIAN_POINT('Ctrl Pts',(1.47174039701251,-3.7965354000586,300.456901424902));
#9031=CARTESIAN_POINT('Ctrl Pts',(3.97921091898969,-0.863470493150105,300.653317708462));
#9032=CARTESIAN_POINT('Ctrl Pts',(2.912940396188,2.84507979848314,300.849733992022));
#9033=CARTESIAN_POINT('Ctrl Pts',(-0.769450467661539,3.99845555198771,301.046150275583));
#9034=CARTESIAN_POINT('Ctrl Pts',(-3.76079560299375,1.56080660361544,301.242566559143));
#9035=CARTESIAN_POINT('Ctrl Pts',(-3.37455913704994,-2.27860734887659,301.438982842703));
#9036=CARTESIAN_POINT('Ctrl Pts',(0.0423788223518119,-4.07159733477241,
301.635399126263));
#9037=CARTESIAN_POINT('Ctrl Pts',(3.421256236785,-2.20787376970116,301.831815409824));
#9038=CARTESIAN_POINT('Ctrl Pts',(3.72749335471555,1.63874772653576,302.028231693384));
#9039=CARTESIAN_POINT('Ctrl Pts',(0.68605771916248,4.01360506615777,302.224647976944));
#9040=CARTESIAN_POINT('Ctrl Pts',(-2.97152837323328,2.78383188193381,302.421064260504));
#9041=CARTESIAN_POINT('Ctrl Pts',(-3.9603760873883,-0.946108909074201,302.617480544064));
#9042=CARTESIAN_POINT('Ctrl Pts',(-1.39239837990148,-3.82634650483378,302.813896827625));
#9043=CARTESIAN_POINT('Ctrl Pts',(2.4260964099369,-3.27013104036704,303.010313111185));
#9044=CARTESIAN_POINT('Ctrl Pts',(4.06570687523191,0.222998733269188,303.206729394745));
#9045=CARTESIAN_POINT('Ctrl Pts',(2.05389402399265,3.51585269576301,303.403145678305));
#9046=CARTESIAN_POINT('Ctrl Pts',(-1.8025270854777,3.65110898740253,303.599561961865));
#9047=CARTESIAN_POINT('Ctrl Pts',(-4.04009333558223,0.507293585058156,303.795978245426));
#9048=CARTESIAN_POINT('Ctrl Pts',(-2.64923982310418,-3.09212375234166,303.992394528986));
#9049=CARTESIAN_POINT('Ctrl Pts',(1.12090367403175,-3.9144954906793,304.188810812546));
#9050=CARTESIAN_POINT('Ctrl Pts',(3.88436049145415,-1.2212476381006,304.385227096106));
#9051=CARTESIAN_POINT('Ctrl Pts',(3.15926127287765,2.56880701797711,304.581643379667));
#9052=CARTESIAN_POINT('Ctrl Pts',(-0.403178846163521,4.05180702950403,304.778059663227));
#9053=CARTESIAN_POINT('Ctrl Pts',(-3.60352487385993,1.89587041543437,304.974475946787));
#9054=CARTESIAN_POINT('Ctrl Pts',(-3.56753031259803,-1.96275979652795,305.170892230348));
#9055=CARTESIAN_POINT('Ctrl Pts',(-0.327535413996504,-4.05861519118165,
305.367308513907));
#9056=CARTESIAN_POINT('Ctrl Pts',(3.20663944956988,-2.50944712830294,305.563724797468));
#9057=CARTESIAN_POINT('Ctrl Pts',(3.86088059109964,1.29352830991355,305.760141081028));
#9058=CARTESIAN_POINT('Ctrl Pts',(1.04774156211884,3.93464263737925,305.956557364589));
#9059=CARTESIAN_POINT('Ctrl Pts',(-2.70656494368751,3.04233932786737,306.152973648148));
#9060=CARTESIAN_POINT('Ctrl Pts',(-4.02969985274476,-0.582931827771558,
306.349389931709));
#9061=CARTESIAN_POINT('Ctrl Pts',(-1.73460718039984,-3.68333889913998,306.545806215269));
#9062=CARTESIAN_POINT('Ctrl Pts',(2.12009592649099,-3.47867745500165,306.742222498829));
#9063=CARTESIAN_POINT('Ctrl Pts',(4.066986376797,-0.14343323816737,306.938682380056));
#9064=CARTESIAN_POINT('Ctrl Pts',(2.93277505209188,2.15491985457359,307.069670166764));
#9065=CARTESIAN_POINT('Ctrl Pts',(2.00558448788872,2.81535315694411,307.135185858951));
#9066=CARTESIAN_POINT('Ctrl Pts',(1.64344736484494,-3.31083465017304,296.863334289856));
#9067=CARTESIAN_POINT('Ctrl Pts',(2.73303855162352,-2.76997835444232,296.928806384376));
#9068=CARTESIAN_POINT('Ctrl Pts',(4.31806526539767,-0.53579067117003,297.059750573417));
#9069=CARTESIAN_POINT('Ctrl Pts',(2.82705787200949,3.31426585664044,297.256166856977));
#9070=CARTESIAN_POINT('Ctrl Pts',(-1.20830520117628,4.1825310018776,297.452583140537));
#9071=CARTESIAN_POINT('Ctrl Pts',(-4.15613426352052,1.29726957454531,297.648999424097));
#9072=CARTESIAN_POINT('Ctrl Pts',(-3.37245777205994,-2.75433400689091,297.845415707658));
#9073=CARTESIAN_POINT('Ctrl Pts',(0.440560090246934,-4.33166004160428,298.041831991218));
#9074=CARTESIAN_POINT('Ctrl Pts',(3.85766129590832,-2.01899074338315,298.238248274778));
#9075=CARTESIAN_POINT('Ctrl Pts',(3.81030211394735,2.10707250760402,298.434664558338));
#9076=CARTESIAN_POINT('Ctrl Pts',(0.34084459659878,4.34070555836707,298.631080841898));
#9077=CARTESIAN_POINT('Ctrl Pts',(-3.43470071493533,2.67596739227649,298.827497125458));
#9078=CARTESIAN_POINT('Ctrl Pts',(-4.12554329970309,-1.3920786942064,299.023913409019));
#9079=CARTESIAN_POINT('Ctrl Pts',(-1.11121762092136,-4.20988835720045,299.220329692579));
#9080=CARTESIAN_POINT('Ctrl Pts',(2.90109320386305,-3.24678792599277,299.416745976139));
#9081=CARTESIAN_POINT('Ctrl Pts',(4.30792493768307,0.63226372230056,299.6131622597));
#9082=CARTESIAN_POINT('Ctrl Pts',(1.84579601545559,3.94347679146638,299.80957854326));
#9083=CARTESIAN_POINT('Ctrl Pts',(-2.27404746424881,3.71304206127767,300.00599482682));
#9084=CARTESIAN_POINT('Ctrl Pts',(-4.35156235295879,0.147913179084922,300.20241111038));
#9085=CARTESIAN_POINT('Ctrl Pts',(-2.52092622284173,-3.55005689521063,300.398827393941));
#9086=CARTESIAN_POINT('Ctrl Pts',(1.57376113943488,-4.05971045520627,300.595243677501));
#9087=CARTESIAN_POINT('Ctrl Pts',(4.25504900363738,-0.923326090611326,300.791659961061));
#9088=CARTESIAN_POINT('Ctrl Pts',(3.11486482691945,3.04230014650195,300.988076244621));
#9089=CARTESIAN_POINT('Ctrl Pts',(-0.822788616242238,4.27562767064716,301.184492528181));
#9090=CARTESIAN_POINT('Ctrl Pts',(-4.02149318274018,1.66900139720936,301.380908811742));
#9091=CARTESIAN_POINT('Ctrl Pts',(-3.60848288420596,-2.43655994288933,301.577325095302));
#9092=CARTESIAN_POINT('Ctrl Pts',(0.0453165136240533,-4.35383962681091,
301.773741378862));
#9093=CARTESIAN_POINT('Ctrl Pts',(3.65841701731566,-2.36092312651506,301.970157662422));
#9094=CARTESIAN_POINT('Ctrl Pts',(3.98588242944266,1.75234538278242,302.166573945982));
#9095=CARTESIAN_POINT('Ctrl Pts',(0.73361509952361,4.29182734603186,302.362990229543));
#9096=CARTESIAN_POINT('Ctrl Pts',(-3.17751411051533,2.97680653694124,302.559406513103));
#9097=CARTESIAN_POINT('Ctrl Pts',(-4.23490854537298,-1.01169298457562,302.755822796663));
#9098=CARTESIAN_POINT('Ctrl Pts',(-1.48891914997317,-4.09158805964929,302.952239080224));
#9099=CARTESIAN_POINT('Ctrl Pts',(2.59427291540787,-3.49681585328236,303.148655363783));
#9100=CARTESIAN_POINT('Ctrl Pts',(4.34754084182337,0.238456959715606,303.345071647344));
#9101=CARTESIAN_POINT('Ctrl Pts',(2.19626953641995,3.75957088342543,303.541487930904));
#9102=CARTESIAN_POINT('Ctrl Pts',(-1.92747789329011,3.90420311345624,303.737904214464));
#9103=CARTESIAN_POINT('Ctrl Pts',(-4.32015177685929,0.542459072313112,303.934320498024));
#9104=CARTESIAN_POINT('Ctrl Pts',(-2.83288458420245,-3.30646913656574,304.130736781585));
#9105=CARTESIAN_POINT('Ctrl Pts',(1.19860448678435,-4.18584751511162,304.327153065145));
#9106=CARTESIAN_POINT('Ctrl Pts',(4.15362356392177,-1.30590427385887,304.523569348705));
#9107=CARTESIAN_POINT('Ctrl Pts',(3.37826061625335,2.74687619352316,304.719985632265));
#9108=CARTESIAN_POINT('Ctrl Pts',(-0.431127121075381,4.33267746164092,304.916401915826));
#9109=CARTESIAN_POINT('Ctrl Pts',(-3.8533204789238,2.02729176373184,305.112818199386));
#9110=CARTESIAN_POINT('Ctrl Pts',(-3.81483078205882,-2.09881790300179,305.309234482946));
#9111=CARTESIAN_POINT('Ctrl Pts',(-0.350240101707314,-4.33995756368946,
305.505650766506));
#9112=CARTESIAN_POINT('Ctrl Pts',(3.42892303843518,-2.6834014884733,305.702067050067));
#9113=CARTESIAN_POINT('Ctrl Pts',(4.12851604169113,1.38319542701492,305.898483333627));
#9114=CARTESIAN_POINT('Ctrl Pts',(1.1203707922814,4.20739125788799,306.094899617187));
#9115=CARTESIAN_POINT('Ctrl Pts',(-2.89418347038547,3.2532336659992,306.291315900747));
#9116=CARTESIAN_POINT('Ctrl Pts',(-4.30903781992354,-0.623340542495704,
306.487732184307));
#9117=CARTESIAN_POINT('Ctrl Pts',(-1.8548497943247,-3.93866719606399,306.684148467868));
#9118=CARTESIAN_POINT('Ctrl Pts',(2.26706054121946,-3.71981866260025,306.880564751428));
#9119=CARTESIAN_POINT('Ctrl Pts',(4.34890903817448,-0.153376000814643,307.077024632655));
#9120=CARTESIAN_POINT('Ctrl Pts',(3.1360744171019,2.3042984568533,307.208012419362));
#9121=CARTESIAN_POINT('Ctrl Pts',(2.14461119318305,3.01051286026928,307.273528111549));
#9122=CARTESIAN_POINT('Ctrl Pts',(1.74998559106762,-3.5254630334674,297.001676542455));
#9123=CARTESIAN_POINT('Ctrl Pts',(2.91021068729191,-2.94954515218115,297.067148636975));
#9124=CARTESIAN_POINT('Ctrl Pts',(4.59798844634642,-0.570523872216909,297.198092826015));
#9125=CARTESIAN_POINT('Ctrl Pts',(3.01032491028253,3.52911667154937,297.394509109576));
#9126=CARTESIAN_POINT('Ctrl Pts',(-1.28663487307368,4.45366802980637,297.590925393136));
#9127=CARTESIAN_POINT('Ctrl Pts',(-4.42556009476432,1.38136645672185,297.787341676696));
#9128=CARTESIAN_POINT('Ctrl Pts',(-3.59108093987892,-2.93288664313347,297.983757960256));
#9129=CARTESIAN_POINT('Ctrl Pts',(0.469119867434461,-4.6124645184034,298.180174243816));
#9130=CARTESIAN_POINT('Ctrl Pts',(4.10773829905756,-2.14987396919328,298.376590527377));
#9131=CARTESIAN_POINT('Ctrl Pts',(4.05730900767332,2.24366572761499,298.573006810937));
#9132=CARTESIAN_POINT('Ctrl Pts',(0.362940210681713,4.62209642042671,298.769423094497));
#9133=CARTESIAN_POINT('Ctrl Pts',(-3.65735884783482,2.8494398292412,298.965839378057));
#9134=CARTESIAN_POINT('Ctrl Pts',(-4.39298603912828,-1.48232167856698,299.162255661618));
#9135=CARTESIAN_POINT('Ctrl Pts',(-1.18325348699944,-4.48279885483234,299.358671945178));
#9136=CARTESIAN_POINT('Ctrl Pts',(3.08915966139477,-3.4572644121619,299.555088228738));
#9137=CARTESIAN_POINT('Ctrl Pts',(4.58719076108503,0.673250891661594,299.751504512298));
#9138=CARTESIAN_POINT('Ctrl Pts',(1.96545170852008,4.19911687553611,299.947920795858));
#9139=CARTESIAN_POINT('Ctrl Pts',(-2.42146501370596,3.9537439684763,300.144337079419));
#9140=CARTESIAN_POINT('Ctrl Pts',(-4.63365701829379,0.157501808493909,300.340753362979));
#9141=CARTESIAN_POINT('Ctrl Pts',(-2.68434795082944,-3.78019311538766,300.537169646539));
#9142=CARTESIAN_POINT('Ctrl Pts',(1.67578188185725,-4.32288551035394,300.733585930099));
#9143=CARTESIAN_POINT('Ctrl Pts',(4.53088708828506,-0.983181688072545,300.93000221366));
#9144=CARTESIAN_POINT('Ctrl Pts',(3.31678925765091,3.23952049452076,301.12641849722));
#9145=CARTESIAN_POINT('Ctrl Pts',(-0.876126764822934,4.55279978930661,301.32283478078));
#9146=CARTESIAN_POINT('Ctrl Pts',(-4.28219076248663,1.77719619080327,301.51925106434));
#9147=CARTESIAN_POINT('Ctrl Pts',(-3.84240663136197,-2.59451253690207,301.7156673479));
#9148=CARTESIAN_POINT('Ctrl Pts',(0.0482542048962955,-4.6360819188494,301.912083631461));
#9149=CARTESIAN_POINT('Ctrl Pts',(3.89557779784632,-2.51397248332897,302.108499915021));
#9150=CARTESIAN_POINT('Ctrl Pts',(4.24427150416976,1.86594303902907,302.304916198581));
#9151=CARTESIAN_POINT('Ctrl Pts',(0.781172479884741,4.57004962590596,302.501332482141));
#9152=CARTESIAN_POINT('Ctrl Pts',(-3.38349984779739,3.16978119194865,302.697748765702));
#9153=CARTESIAN_POINT('Ctrl Pts',(-4.50944100335765,-1.07727706007705,302.894165049262));
#9154=CARTESIAN_POINT('Ctrl Pts',(-1.58543992004487,-4.3568296144648,303.090581332822));
#9155=CARTESIAN_POINT('Ctrl Pts',(2.76244942087883,-3.72350066619769,303.286997616382));
#9156=CARTESIAN_POINT('Ctrl Pts',(4.62937480841483,0.253915186162026,303.483413899943));
#9157=CARTESIAN_POINT('Ctrl Pts',(2.33864504884725,4.00328907108784,303.679830183503));
#9158=CARTESIAN_POINT('Ctrl Pts',(-2.05242870110252,4.15729723950994,303.876246467063));
#9159=CARTESIAN_POINT('Ctrl Pts',(-4.60021021813634,0.577624559568071,304.072662750623));
#9160=CARTESIAN_POINT('Ctrl Pts',(-3.01652934530071,-3.52081452078982,304.269079034184));
#9161=CARTESIAN_POINT('Ctrl Pts',(1.27630529953692,-4.45719953954392,304.465495317743));
#9162=CARTESIAN_POINT('Ctrl Pts',(4.42288663638938,-1.39056090961712,304.661911601304));
#9163=CARTESIAN_POINT('Ctrl Pts',(3.59725995962907,2.9249453690692,304.858327884864));
#9164=CARTESIAN_POINT('Ctrl Pts',(-0.459075395987237,4.61354789377779,305.054744168424));
#9165=CARTESIAN_POINT('Ctrl Pts',(-4.10311608398768,2.15871311202932,305.251160451984));
#9166=CARTESIAN_POINT('Ctrl Pts',(-4.0621312515196,-2.23487600947561,305.447576735545));
#9167=CARTESIAN_POINT('Ctrl Pts',(-0.372944789418124,-4.62129993619727,
305.643993019105));
#9168=CARTESIAN_POINT('Ctrl Pts',(3.6512066273005,-2.85735584864364,305.840409302665));
#9169=CARTESIAN_POINT('Ctrl Pts',(4.39615149228261,1.47286254411629,306.036825586225));
#9170=CARTESIAN_POINT('Ctrl Pts',(1.19300002244395,4.48013987839675,306.233241869786));
#9171=CARTESIAN_POINT('Ctrl Pts',(-3.08180199708344,3.46412800413103,306.429658153346));
#9172=CARTESIAN_POINT('Ctrl Pts',(-4.58837578710231,-0.663749257219848,
306.626074436906));
#9173=CARTESIAN_POINT('Ctrl Pts',(-1.97509240824956,-4.19399549298801,306.822490720466));
#9174=CARTESIAN_POINT('Ctrl Pts',(2.41402515594792,-3.96095987019886,307.018907004026));
#9175=CARTESIAN_POINT('Ctrl Pts',(4.63083169955196,-0.163318763461907,307.215366885254));
#9176=CARTESIAN_POINT('Ctrl Pts',(3.33937378211193,2.45367705913301,307.346354671961));
#9177=CARTESIAN_POINT('Ctrl Pts',(2.28363789847738,3.20567256359444,307.411870364148));
#9178=CARTESIAN_POINT('Ctrl Pts',(1.75295277484312,-3.52741701688456,307.));
#9179=CARTESIAN_POINT('Ctrl Pts',(1.84997325411491,-3.46888291556181,307.));
#9180=CARTESIAN_POINT('Ctrl Pts',(1.94403576147925,-3.40606933859778,307.));
#9181=CARTESIAN_POINT('Ctrl Pts',(2.03481898164511,-3.33898497869234,307.));
#9182=CARTESIAN_POINT('Ctrl Pts',(2.13159970155574,-3.26746875978613,307.));
#9183=CARTESIAN_POINT('Ctrl Pts',(2.2246543845738,-3.19109872939616,307.));
#9184=CARTESIAN_POINT('Ctrl Pts',(2.31382658373371,-3.110286348705,307.));
#9185=CARTESIAN_POINT('Ctrl Pts',(2.40455794825776,-3.02806097308767,307.));
#9186=CARTESIAN_POINT('Ctrl Pts',(2.49127034422638,-2.94123570859823,307.));
#9187=CARTESIAN_POINT('Ctrl Pts',(2.57375432305174,-2.85021295057718,307.));
#9188=CARTESIAN_POINT('Ctrl Pts',(2.65623830187711,-2.75919019255613,307.));
#9189=CARTESIAN_POINT('Ctrl Pts',(2.73449421814026,-2.66396901625497,307.));
#9190=CARTESIAN_POINT('Ctrl Pts',(2.80826230895727,-2.56493446116125,307.));
#9191=CARTESIAN_POINT('Ctrl Pts',(2.81895233475812,-2.55058297209054,307.));
#9192=CARTESIAN_POINT('Ctrl Pts',(2.82954802439101,-2.53615138610789,307.));
#9193=CARTESIAN_POINT('Ctrl Pts',(2.84004849278268,-2.52164086262617,307.));
#9194=CARTESIAN_POINT('Ctrl Pts',(2.85054939974663,-2.5071297330845,307.));
#9195=CARTESIAN_POINT('Ctrl Pts',(2.86095084159264,-2.49254545377891,307.));
#9196=CARTESIAN_POINT('Ctrl Pts',(2.87124786780565,-2.47789562877494,307.));
#9197=CARTESIAN_POINT('Ctrl Pts',(2.94008136874243,-2.37996456379809,307.));
#9198=CARTESIAN_POINT('Ctrl Pts',(3.00431541770822,-2.27902010980789,307.));
#9199=CARTESIAN_POINT('Ctrl Pts',(3.0637933403493,-2.17545767538768,307.));
#9200=CARTESIAN_POINT('Ctrl Pts',(3.12323362815573,-2.07196077040969,307.));
#9201=CARTESIAN_POINT('Ctrl Pts',(3.17792410148909,-1.96584830416904,307.));
#9202=CARTESIAN_POINT('Ctrl Pts',(3.2276602081122,-1.85749568873033,307.));
#9203=CARTESIAN_POINT('Ctrl Pts',(3.27649169173924,-1.75111384008994,307.));
#9204=CARTESIAN_POINT('Ctrl Pts',(3.3205475227483,-1.64257176239661,307.));
#9205=CARTESIAN_POINT('Ctrl Pts',(3.35958475361651,-1.5322189723795,307.));
#9206=CARTESIAN_POINT('Ctrl Pts',(3.37957181235439,-1.47571835369042,307.));
#9207=CARTESIAN_POINT('Ctrl Pts',(3.3982424616149,-1.4187430500264,307.));
#9208=CARTESIAN_POINT('Ctrl Pts',(3.41555877354041,-1.36134041511221,307.));
#9209=CARTESIAN_POINT('Ctrl Pts',(3.42952961902185,-1.3150278200248,307.));
#9210=CARTESIAN_POINT('Ctrl Pts',(3.44261881817217,-1.26843706414811,307.));
#9211=CARTESIAN_POINT('Ctrl Pts',(3.45480465835639,-1.22159339689648,307.));
#9212=CARTESIAN_POINT('Ctrl Pts',(3.45882230994349,-1.20614911638451,307.));
#9213=CARTESIAN_POINT('Ctrl Pts',(3.46274127720411,-1.19067897371837,307.));
#9214=CARTESIAN_POINT('Ctrl Pts',(3.46655813556577,-1.17519536513956,307.));
#9215=CARTESIAN_POINT('Ctrl Pts',(3.49407224813524,-1.06358060004956,307.));
#9216=CARTESIAN_POINT('Ctrl Pts',(3.51632768255355,-0.95110272169328,307.));
#9217=CARTESIAN_POINT('Ctrl Pts',(3.53314119320375,-0.83810325534612,307.));
#9218=CARTESIAN_POINT('Ctrl Pts',(3.54951998604572,-0.728025420380012,307.));
#9219=CARTESIAN_POINT('Ctrl Pts',(3.56073462608323,-0.617451900568752,307.));
#9220=CARTESIAN_POINT('Ctrl Pts',(3.56656734873009,-0.506699353783957,307.));
#9221=CARTESIAN_POINT('Ctrl Pts',(3.57237373653643,-0.39644685660448,307.));
#9222=CARTESIAN_POINT('Ctrl Pts',(3.57284686430163,-0.286016286590276,307.));
#9223=CARTESIAN_POINT('Ctrl Pts',(3.56772180702459,-0.175731148929752,307.));
#9224=CARTESIAN_POINT('Ctrl Pts',(3.56700386529454,-0.160281896706627,307.));
#9225=CARTESIAN_POINT('Ctrl Pts',(3.56617598339815,-0.144835525589673,307.));
#9226=CARTESIAN_POINT('Ctrl Pts',(3.56523735115947,-0.129392953786932,307.));
#9227=CARTESIAN_POINT('Ctrl Pts',(3.56100709348304,-0.059795879213749,307.));
#9228=CARTESIAN_POINT('Ctrl Pts',(3.55452777976943,0.00972434142671849,
307.));
#9229=CARTESIAN_POINT('Ctrl Pts',(3.54583829760014,0.0790805148444869,307.));
#9230=CARTESIAN_POINT('Ctrl Pts',(3.54239356966496,0.106575035621981,307.));
#9231=CARTESIAN_POINT('Ctrl Pts',(3.53860144372464,0.134043731144043,307.));
#9232=CARTESIAN_POINT('Ctrl Pts',(3.53446410048778,0.161480979003646,307.));
#9233=CARTESIAN_POINT('Ctrl Pts',(3.53224607865982,0.176190035315359,307.));
#9234=CARTESIAN_POINT('Ctrl Pts',(3.52992929936332,0.190886746487658,307.));
#9235=CARTESIAN_POINT('Ctrl Pts',(3.52751569347095,0.20556195564389,307.));
#9236=CARTESIAN_POINT('Ctrl Pts',(3.50945137554655,0.315396641018207,307.));
#9237=CARTESIAN_POINT('Ctrl Pts',(3.48594688677709,0.424166839182885,307.));
#9238=CARTESIAN_POINT('Ctrl Pts',(3.45725530888715,0.531549258372834,307.));
#9239=CARTESIAN_POINT('Ctrl Pts',(3.42830185569478,0.639911784115604,307.));
#9240=CARTESIAN_POINT('Ctrl Pts',(3.39406567191996,0.746861877867126,307.));
#9241=CARTESIAN_POINT('Ctrl Pts',(3.3547574652526,0.852046538270801,307.));
#9242=CARTESIAN_POINT('Ctrl Pts',(3.31573092144832,0.956477498236013,307.));
#9243=CARTESIAN_POINT('Ctrl Pts',(3.27170416736303,1.05916893424089,307.));
#9244=CARTESIAN_POINT('Ctrl Pts',(3.2228436680777,1.15974389177418,307.));
#9245=CARTESIAN_POINT('Ctrl Pts',(3.18636005117348,1.23484214648859,307.));
#9246=CARTESIAN_POINT('Ctrl Pts',(3.14718054401227,1.30875978471779,307.));
#9247=CARTESIAN_POINT('Ctrl Pts',(3.10536284645011,1.38132480753957,307.));
#9248=CARTESIAN_POINT('Ctrl Pts',(3.09616761950596,1.39728101488604,307.));
#9249=CARTESIAN_POINT('Ctrl Pts',(3.08684392630523,1.41317322762995,307.));
#9250=CARTESIAN_POINT('Ctrl Pts',(3.07739507132796,1.42899493090577,307.));
#9251=CARTESIAN_POINT('Ctrl Pts',(3.0208896010318,1.52361092264631,307.));
#9252=CARTESIAN_POINT('Ctrl Pts',(2.9600630238022,1.61545588204263,307.));
#9253=CARTESIAN_POINT('Ctrl Pts',(2.89510248933946,1.70417986891544,307.));
#9254=CARTESIAN_POINT('Ctrl Pts',(2.83126422465857,1.79137104436335,307.));
#9255=CARTESIAN_POINT('Ctrl Pts',(2.76343297954024,1.87554869262835,307.));
#9256=CARTESIAN_POINT('Ctrl Pts',(2.69175573855431,1.95634128855535,307.));
#9257=CARTESIAN_POINT('Ctrl Pts',(2.66214252473009,1.98972048096971,307.));
#9258=CARTESIAN_POINT('Ctrl Pts',(2.6318725241643,2.02252136225033,307.));
#9259=CARTESIAN_POINT('Ctrl Pts',(2.60095491029651,2.05471539319883,307.));
#9260=CARTESIAN_POINT('Ctrl Pts',(2.58369001395723,2.07269306150938,307.));
#9261=CARTESIAN_POINT('Ctrl Pts',(2.56622316200388,2.09048147053325,307.));
#9262=CARTESIAN_POINT('Ctrl Pts',(2.54855587341939,2.10807544530337,307.));
#9263=CARTESIAN_POINT('Ctrl Pts',(2.5342735759129,2.12229847566746,307.));
#9264=CARTESIAN_POINT('Ctrl Pts',(2.51986594619975,2.1363887535211,307.));
#9265=CARTESIAN_POINT('Ctrl Pts',(2.50533827639883,2.15033988947171,307.));
#9266=CARTESIAN_POINT('Ctrl Pts',(2.42916611523439,2.22348914125257,307.));
#9267=CARTESIAN_POINT('Ctrl Pts',(2.34965953843726,2.2928529993755,307.));
#9268=CARTESIAN_POINT('Ctrl Pts',(2.26696419899973,2.35808473048493,307.));
#9269=CARTESIAN_POINT('Ctrl Pts',(2.18652064639967,2.42154020727947,307.));
#9270=CARTESIAN_POINT('Ctrl Pts',(2.10305907939019,2.4810858444035,307.));
#9271=CARTESIAN_POINT('Ctrl Pts',(2.0166946005239,2.53635740752467,307.));
#9272=CARTESIAN_POINT('Ctrl Pts',(1.96919770923866,2.56675448117339,307.));
#9273=CARTESIAN_POINT('Ctrl Pts',(1.92082252976015,2.59585801512022,307.));
#9274=CARTESIAN_POINT('Ctrl Pts',(1.87158653173908,2.62360084935054,307.));
#9275=CARTESIAN_POINT('Ctrl Pts',(1.8756224353083,2.62673419576125,297.));
#9276=CARTESIAN_POINT('Ctrl Pts',(1.95765324669421,2.58118494599767,297.));
#9277=CARTESIAN_POINT('Ctrl Pts',(2.03738954822689,2.53196003294659,297.));
#9278=CARTESIAN_POINT('Ctrl Pts',(2.11454810562212,2.47911826575738,297.));
#9279=CARTESIAN_POINT('Ctrl Pts',(2.19986126849811,2.42069184562907,297.));
#9280=CARTESIAN_POINT('Ctrl Pts',(2.28202434826617,2.35784481146803,297.));
#9281=CARTESIAN_POINT('Ctrl Pts',(2.36094618439224,2.2909673251695,297.));
#9282=CARTESIAN_POINT('Ctrl Pts',(2.40953886514322,2.24979042786644,297.));
#9283=CARTESIAN_POINT('Ctrl Pts',(2.45690244537228,2.20708458165014,297.));
#9284=CARTESIAN_POINT('Ctrl Pts',(2.50301134826845,2.1629320969333,297.));
#9285=CARTESIAN_POINT('Ctrl Pts',(2.51681233550409,2.14971669080293,297.));
#9286=CARTESIAN_POINT('Ctrl Pts',(2.53050089340508,2.13637164146357,297.));
#9287=CARTESIAN_POINT('Ctrl Pts',(2.54407626948497,2.12289905300282,297.));
#9288=CARTESIAN_POINT('Ctrl Pts',(2.55828158733512,2.10880129245292,297.));
#9289=CARTESIAN_POINT('Ctrl Pts',(2.5723574584733,2.09456930457899,297.));
#9290=CARTESIAN_POINT('Ctrl Pts',(2.58629903742493,2.08021029150632,297.));
#9291=CARTESIAN_POINT('Ctrl Pts',(2.66022714209237,2.00406865611193,297.));
#9292=CARTESIAN_POINT('Ctrl Pts',(2.73041918130771,1.92432121396313,297.));
#9293=CARTESIAN_POINT('Ctrl Pts',(2.79678221780539,1.84137617106676,297.));
#9294=CARTESIAN_POINT('Ctrl Pts',(2.86479487312921,1.75636932220854,297.));
#9295=CARTESIAN_POINT('Ctrl Pts',(2.92878637777531,1.66800343120733,297.));
#9296=CARTESIAN_POINT('Ctrl Pts',(2.98862845706434,1.57667128181542,297.));
#9297=CARTESIAN_POINT('Ctrl Pts',(3.01039937231069,1.54344408604781,297.));
#9298=CARTESIAN_POINT('Ctrl Pts',(3.03162078208611,1.50982389187596,297.));
#9299=CARTESIAN_POINT('Ctrl Pts',(3.05228537984315,1.47582834566168,297.));
#9300=CARTESIAN_POINT('Ctrl Pts',(3.06150211787551,1.46066579338712,297.));
#9301=CARTESIAN_POINT('Ctrl Pts',(3.07060854300814,1.44542777629857,297.));
#9302=CARTESIAN_POINT('Ctrl Pts',(3.07960253589492,1.43011825637885,297.));
#9303=CARTESIAN_POINT('Ctrl Pts',(3.08792329757299,1.41595470652269,297.));
#9304=CARTESIAN_POINT('Ctrl Pts',(3.09614466223841,1.40173534905011,297.));
#9305=CARTESIAN_POINT('Ctrl Pts',(3.10426515935106,1.3874636942554,297.));
#9306=CARTESIAN_POINT('Ctrl Pts',(3.1594813980601,1.29042196306753,297.));
#9307=CARTESIAN_POINT('Ctrl Pts',(3.21005549239299,1.1909335558491,297.));
#9308=CARTESIAN_POINT('Ctrl Pts',(3.25588594072735,1.08943234816672,297.));
#9309=CARTESIAN_POINT('Ctrl Pts',(3.30225956579053,0.986728160894039,297.));
#9310=CARTESIAN_POINT('Ctrl Pts',(3.34377699428959,0.881962476690267,297.));
#9311=CARTESIAN_POINT('Ctrl Pts',(3.38029857606622,0.775543280911798,297.));
#9312=CARTESIAN_POINT('Ctrl Pts',(3.41675039082397,0.669327377260349,297.));
#9313=CARTESIAN_POINT('Ctrl Pts',(3.44822592417807,0.561463458521685,297.));
#9314=CARTESIAN_POINT('Ctrl Pts',(3.47454435174328,0.452327636711442,297.));
#9315=CARTESIAN_POINT('Ctrl Pts',(3.49204141362862,0.379771773585114,297.));
#9316=CARTESIAN_POINT('Ctrl Pts',(3.50725822641119,0.30665315370922,297.));
#9317=CARTESIAN_POINT('Ctrl Pts',(3.5201296905142,0.233077758113266,297.));
#9318=CARTESIAN_POINT('Ctrl Pts',(3.52324750007939,0.215255848319997,297.));
#9319=CARTESIAN_POINT('Ctrl Pts',(3.5262276519985,0.197407126484436,297.));
#9320=CARTESIAN_POINT('Ctrl Pts',(3.52906912818209,0.179533080052531,297.));
#9321=CARTESIAN_POINT('Ctrl Pts',(3.53130134307825,0.165491536107698,297.));
#9322=CARTESIAN_POINT('Ctrl Pts',(3.53344765401367,0.151436138428793,297.));
#9323=CARTESIAN_POINT('Ctrl Pts',(3.53550638032799,0.137376848547553,297.));
#9324=CARTESIAN_POINT('Ctrl Pts',(3.55229157977818,0.0227487004818831,297.));
#9325=CARTESIAN_POINT('Ctrl Pts',(3.56328560075331,-0.0923062269536467,
297.));
#9326=CARTESIAN_POINT('Ctrl Pts',(3.56835208320539,-0.207362631195156,297.));
#9327=CARTESIAN_POINT('Ctrl Pts',(3.57176836951555,-0.284944192450943,297.));
#9328=CARTESIAN_POINT('Ctrl Pts',(3.57248877647768,-0.362527172824792,297.));
#9329=CARTESIAN_POINT('Ctrl Pts',(3.57045975383798,-0.439987598678934,297.));
#9330=CARTESIAN_POINT('Ctrl Pts',(3.5675206935761,-0.55218982601893,297.));
#9331=CARTESIAN_POINT('Ctrl Pts',(3.55881561640657,-0.664134903948192,297.));
#9332=CARTESIAN_POINT('Ctrl Pts',(3.54461270917885,-0.77552871598842,297.));
#9333=CARTESIAN_POINT('Ctrl Pts',(3.53040980195112,-0.886922528028648,297.));
#9334=CARTESIAN_POINT('Ctrl Pts',(3.51070879796927,-0.997765757946331,297.));
#9335=CARTESIAN_POINT('Ctrl Pts',(3.48572532531809,-1.10776627052454,297.));
#9336=CARTESIAN_POINT('Ctrl Pts',(3.48023441116192,-1.13194238807772,297.));
#9337=CARTESIAN_POINT('Ctrl Pts',(3.47448813976633,-1.15607778380368,297.));
#9338=CARTESIAN_POINT('Ctrl Pts',(3.46848847990599,-1.18016931768953,297.));
#9339=CARTESIAN_POINT('Ctrl Pts',(3.46260502329978,-1.20379423935069,297.));
#9340=CARTESIAN_POINT('Ctrl Pts',(3.4564769563925,-1.22737979626238,297.));
#9341=CARTESIAN_POINT('Ctrl Pts',(3.4501156361031,-1.25088950819066,297.));
#9342=CARTESIAN_POINT('Ctrl Pts',(3.41996601999333,-1.3623143000959,297.));
#9343=CARTESIAN_POINT('Ctrl Pts',(3.38454132687335,-1.47220190710762,297.));
#9344=CARTESIAN_POINT('Ctrl Pts',(3.34415317658468,-1.58024732335799,297.));
#9345=CARTESIAN_POINT('Ctrl Pts',(3.30309881449456,-1.69007497352804,297.));
#9346=CARTESIAN_POINT('Ctrl Pts',(3.25691572359613,-1.7979998724566,297.));
#9347=CARTESIAN_POINT('Ctrl Pts',(3.20587623943613,-1.90370463532879,297.));
#9348=CARTESIAN_POINT('Ctrl Pts',(3.15419187937227,-2.01074496135608,297.));
#9349=CARTESIAN_POINT('Ctrl Pts',(3.09752739549888,-2.11550950113078,297.));
#9350=CARTESIAN_POINT('Ctrl Pts',(3.03611285331182,-2.21766010847631,297.));
#9351=CARTESIAN_POINT('Ctrl Pts',(2.98506113429581,-2.30257426590232,297.));
#9352=CARTESIAN_POINT('Ctrl Pts',(2.93072608037477,-2.38568227462021,297.));
#9353=CARTESIAN_POINT('Ctrl Pts',(2.87321456924896,-2.4667792858147,297.));
#9354=CARTESIAN_POINT('Ctrl Pts',(2.86373431057747,-2.48014740340644,297.));
#9355=CARTESIAN_POINT('Ctrl Pts',(2.85416769185057,-2.49346084869992,297.));
#9356=CARTESIAN_POINT('Ctrl Pts',(2.8445151364034,-2.50671866846762,297.));
#9357=CARTESIAN_POINT('Ctrl Pts',(2.83449211073775,-2.52048533041839,297.));
#9358=CARTESIAN_POINT('Ctrl Pts',(2.8243817964104,-2.5341846142502,297.));
#9359=CARTESIAN_POINT('Ctrl Pts',(2.81418689372382,-2.54781310286705,297.));
#9360=CARTESIAN_POINT('Ctrl Pts',(2.74077335186671,-2.64595191304319,297.));
#9361=CARTESIAN_POINT('Ctrl Pts',(2.66294685987612,-2.74046301248844,297.));
#9362=CARTESIAN_POINT('Ctrl Pts',(2.58099765137135,-2.83101116490618,297.));
#9363=CARTESIAN_POINT('Ctrl Pts',(2.49890799991651,-2.92171449697581,297.));
#9364=CARTESIAN_POINT('Ctrl Pts',(2.41268110510993,-3.00844211791462,297.));
#9365=CARTESIAN_POINT('Ctrl Pts',(2.32255885079943,-3.09084082744064,297.));
#9366=CARTESIAN_POINT('Ctrl Pts',(2.23414169014168,-3.17168057111874,297.));
#9367=CARTESIAN_POINT('Ctrl Pts',(2.14197466942637,-3.2483543632461,297.));
#9368=CARTESIAN_POINT('Ctrl Pts',(2.04624509609143,-3.3205018093572,297.));
#9369=CARTESIAN_POINT('Ctrl Pts',(1.95056982624481,-3.39260832916037,297.));
#9370=CARTESIAN_POINT('Ctrl Pts',(1.85133567663837,-3.46019442836626,297.));
#9371=CARTESIAN_POINT('Ctrl Pts',(1.74869447533122,-3.52286199445083,297.));
#9372=CARTESIAN_POINT('Origin',(-5.160062080289E-16,2.1385152528819E-16,
297.));
#9373=CARTESIAN_POINT('Ctrl Pts',(-1.81480609505069,-3.48926465567845,297.));
#9374=CARTESIAN_POINT('Ctrl Pts',(-1.89001899604713,-3.44184200468758,297.));
#9375=CARTESIAN_POINT('Ctrl Pts',(-1.96341204602375,-3.39175063166926,297.));
#9376=CARTESIAN_POINT('Ctrl Pts',(-2.03481909388391,-3.33898430436496,297.));
#9377=CARTESIAN_POINT('Ctrl Pts',(-2.1330728566162,-3.26637956353652,297.));
#9378=CARTESIAN_POINT('Ctrl Pts',(-2.22756835178525,-3.18871116509068,297.));
#9379=CARTESIAN_POINT('Ctrl Pts',(-2.31811726774695,-3.10639114222592,297.));
#9380=CARTESIAN_POINT('Ctrl Pts',(-2.38810348676451,-3.04276512209577,297.));
#9381=CARTESIAN_POINT('Ctrl Pts',(-2.45573128771564,-2.97635938300247,297.));
#9382=CARTESIAN_POINT('Ctrl Pts',(-2.5208950964127,-2.90735384839687,297.));
#9383=CARTESIAN_POINT('Ctrl Pts',(-2.53489034792619,-2.89253350821206,297.));
#9384=CARTESIAN_POINT('Ctrl Pts',(-2.54877166048973,-2.8775933504051,297.));
#9385=CARTESIAN_POINT('Ctrl Pts',(-2.56252866764529,-2.86254555233852,297.));
#9386=CARTESIAN_POINT('Ctrl Pts',(-2.64400028421257,-2.77342962614914,297.));
#9387=CARTESIAN_POINT('Ctrl Pts',(-2.7212018811122,-2.68045059264905,297.));
#9388=CARTESIAN_POINT('Ctrl Pts',(-2.79395934645943,-2.58401337193643,297.));
#9389=CARTESIAN_POINT('Ctrl Pts',(-2.86676825659545,-2.4875079631358,297.));
#9390=CARTESIAN_POINT('Ctrl Pts',(-2.93512707424484,-2.38753858357703,297.));
#9391=CARTESIAN_POINT('Ctrl Pts',(-2.99881400156226,-2.28449030256758,297.));
#9392=CARTESIAN_POINT('Ctrl Pts',(-3.03468906634645,-2.2264428521279,297.));
#9393=CARTESIAN_POINT('Ctrl Pts',(-3.06908080882254,-2.16741813460255,297.));
#9394=CARTESIAN_POINT('Ctrl Pts',(-3.10194238684353,-2.10748369667657,297.));
#9395=CARTESIAN_POINT('Ctrl Pts',(-3.11090507486663,-2.09113713934972,297.));
#9396=CARTESIAN_POINT('Ctrl Pts',(-3.11975419834814,-2.07472221701618,297.));
#9397=CARTESIAN_POINT('Ctrl Pts',(-3.12848132276822,-2.05825471066704,297.));
#9398=CARTESIAN_POINT('Ctrl Pts',(-3.18408615702895,-1.95333206751959,297.));
#9399=CARTESIAN_POINT('Ctrl Pts',(-3.23481830075119,-1.84613953636477,297.));
#9400=CARTESIAN_POINT('Ctrl Pts',(-3.28051179803537,-1.73705586719653,297.));
#9401=CARTESIAN_POINT('Ctrl Pts',(-3.32587389771413,-1.62876334050814,297.));
#9402=CARTESIAN_POINT('Ctrl Pts',(-3.36627038976648,-1.51860614079287,297.));
#9403=CARTESIAN_POINT('Ctrl Pts',(-3.40148946203064,-1.40694277436367,297.));
#9404=CARTESIAN_POINT('Ctrl Pts',(-3.43581642062762,-1.29810788719042,297.));
#9405=CARTESIAN_POINT('Ctrl Pts',(-3.4652249691995,-1.18784142279203,297.));
#9406=CARTESIAN_POINT('Ctrl Pts',(-3.48947021542989,-1.07647566774693,297.));
#9407=CARTESIAN_POINT('Ctrl Pts',(-3.50639009325733,-0.998757547187614,
297.));
#9408=CARTESIAN_POINT('Ctrl Pts',(-3.52079437228538,-0.920504057101386,
297.));
#9409=CARTESIAN_POINT('Ctrl Pts',(-3.53258497104414,-0.841831067608438,
297.));
#9410=CARTESIAN_POINT('Ctrl Pts',(-3.53678136293646,-0.813830564664707,
297.));
#9411=CARTESIAN_POINT('Ctrl Pts',(-3.54064655877754,-0.785776955752405,
297.));
#9412=CARTESIAN_POINT('Ctrl Pts',(-3.54417574632832,-0.757675588895275,
297.));
#9413=CARTESIAN_POINT('Ctrl Pts',(-3.54658855565722,-0.738463450369874,
297.));
#9414=CARTESIAN_POINT('Ctrl Pts',(-3.54884441401843,-0.719227172536132,
297.));
#9415=CARTESIAN_POINT('Ctrl Pts',(-3.55093961590336,-0.699990393966351,
297.));
#9416=CARTESIAN_POINT('Ctrl Pts',(-3.56306129535751,-0.588697031149804,
297.));
#9417=CARTESIAN_POINT('Ctrl Pts',(-3.56983156372365,-0.477223248990884,
297.));
#9418=CARTESIAN_POINT('Ctrl Pts',(-3.57106196810248,-0.365887824980338,
297.));
#9419=CARTESIAN_POINT('Ctrl Pts',(-3.57193436072074,-0.286947759642042,
297.));
#9420=CARTESIAN_POINT('Ctrl Pts',(-3.57002072133686,-0.208077152176203,
297.));
#9421=CARTESIAN_POINT('Ctrl Pts',(-3.56523803549323,-0.129391528174488,
297.));
#9422=CARTESIAN_POINT('Ctrl Pts',(-3.5583383934639,-0.0158773530401223,
297.));
#9423=CARTESIAN_POINT('Ctrl Pts',(-3.54546949243385,0.0972530756745339,
297.));
#9424=CARTESIAN_POINT('Ctrl Pts',(-3.52684415090893,0.209634660021319,297.));
#9425=CARTESIAN_POINT('Ctrl Pts',(-3.50828799890508,0.321598768640824,297.));
#9426=CARTESIAN_POINT('Ctrl Pts',(-3.48401750053588,0.432820345922119,297.));
#9427=CARTESIAN_POINT('Ctrl Pts',(-3.45419980180639,0.542910574102145,297.));
#9428=CARTESIAN_POINT('Ctrl Pts',(-3.44899732296649,0.562118699041036,297.));
#9429=CARTESIAN_POINT('Ctrl Pts',(-3.44362588238673,0.581292298646908,297.));
#9430=CARTESIAN_POINT('Ctrl Pts',(-3.43808625278056,0.600429194129876,297.));
#9431=CARTESIAN_POINT('Ctrl Pts',(-3.43195656329836,0.621604477551889,297.));
#9432=CARTESIAN_POINT('Ctrl Pts',(-3.42562070782981,0.642735019730582,297.));
#9433=CARTESIAN_POINT('Ctrl Pts',(-3.41908837506188,0.663791541218352,297.));
#9434=CARTESIAN_POINT('Ctrl Pts',(-3.38609238768416,0.770151817387931,297.));
#9435=CARTESIAN_POINT('Ctrl Pts',(-3.34803954138042,0.874794555533513,297.));
#9436=CARTESIAN_POINT('Ctrl Pts',(-3.30516552460409,0.977392176481827,297.));
#9437=CARTESIAN_POINT('Ctrl Pts',(-3.26223302087613,1.08012975684018,297.));
#9438=CARTESIAN_POINT('Ctrl Pts',(-3.2144655987723,1.1808173900939,297.));
#9439=CARTESIAN_POINT('Ctrl Pts',(-3.16205541704689,1.27909866910512,297.));
#9440=CARTESIAN_POINT('Ctrl Pts',(-3.11058511725006,1.37561745092552,297.));
#9441=CARTESIAN_POINT('Ctrl Pts',(-3.0546364418454,1.46981598829565,297.));
#9442=CARTESIAN_POINT('Ctrl Pts',(-2.99435779069831,1.5613205369265,297.));
#9443=CARTESIAN_POINT('Ctrl Pts',(-2.94203711605949,1.64074467176993,297.));
#9444=CARTESIAN_POINT('Ctrl Pts',(-2.88645356779812,1.71813888458468,297.));
#9445=CARTESIAN_POINT('Ctrl Pts',(-2.82768844580675,1.79323101137441,297.));
#9446=CARTESIAN_POINT('Ctrl Pts',(-2.81808060469522,1.80550824655191,297.));
#9447=CARTESIAN_POINT('Ctrl Pts',(-2.80839358794498,1.8177163353674,297.));
#9448=CARTESIAN_POINT('Ctrl Pts',(-2.7986290191487,1.8298530527289,297.));
#9449=CARTESIAN_POINT('Ctrl Pts',(-2.73124593785801,1.91360579487594,297.));
#9450=CARTESIAN_POINT('Ctrl Pts',(-2.66015654899076,1.99398334177554,297.));
#9451=CARTESIAN_POINT('Ctrl Pts',(-2.58553694647172,2.07066463497472,297.));
#9452=CARTESIAN_POINT('Ctrl Pts',(-2.51196902352116,2.14626519138864,297.));
#9453=CARTESIAN_POINT('Ctrl Pts',(-2.43496910430356,2.21827345872741,297.));
#9454=CARTESIAN_POINT('Ctrl Pts',(-2.35467764042612,2.28634088207263,297.));
#9455=CARTESIAN_POINT('Ctrl Pts',(-2.27685756127256,2.35231317871164,297.));
#9456=CARTESIAN_POINT('Ctrl Pts',(-2.19594490517152,2.41458378331137,297.));
#9457=CARTESIAN_POINT('Ctrl Pts',(-2.11204909346534,2.47279110641631,297.));
#9458=CARTESIAN_POINT('Ctrl Pts',(-2.03442340485464,2.5266481875544,297.));
#9459=CARTESIAN_POINT('Ctrl Pts',(-1.95424336070402,2.57702649732872,297.));
#9460=CARTESIAN_POINT('Ctrl Pts',(-1.87158653173917,2.62360084935051,297.));
#9461=CARTESIAN_POINT('Ctrl Pts',(-2.28393822976682,3.20620192138523,296.587776945939));
#9462=CARTESIAN_POINT('Ctrl Pts',(-3.33986665587357,2.45409656577389,296.653293691435));
#9463=CARTESIAN_POINT('Ctrl Pts',(-4.63155725221788,-0.163320862335666,
296.784282531451));
#9464=CARTESIAN_POINT('Ctrl Pts',(-2.41439620993322,-3.96156897885787,296.980743465989));
#9465=CARTESIAN_POINT('Ctrl Pts',(1.97539585625794,-4.19463976840236,297.177159749549));
#9466=CARTESIAN_POINT('Ctrl Pts',(4.58908114628793,-0.663851457345065,297.373576033109));
#9467=CARTESIAN_POINT('Ctrl Pts',(3.08227572751309,3.46466062107002,297.569992316669));
#9468=CARTESIAN_POINT('Ctrl Pts',(-1.19318341285997,4.48082852509293,297.766408600229));
#9469=CARTESIAN_POINT('Ctrl Pts',(-4.396827278237,1.47308898323638,297.96282488379));
#9470=CARTESIAN_POINT('Ctrl Pts',(-3.65176790097364,-2.85779510217247,298.15924116735));
#9471=CARTESIAN_POINT('Ctrl Pts',(0.373002120370937,-4.62201032653495,298.35565745091));
#9472=CARTESIAN_POINT('Ctrl Pts',(4.06275569155672,-2.23521956363059,298.55207373447));
#9473=CARTESIAN_POINT('Ctrl Pts',(4.10374682531429,2.15904495645791,298.748490018031));
#9474=CARTESIAN_POINT('Ctrl Pts',(0.459145965957643,4.61425709863479,298.944906301591));
#9475=CARTESIAN_POINT('Ctrl Pts',(-3.59781293903473,2.92539499921914,299.141322585151));
#9476=CARTESIAN_POINT('Ctrl Pts',(-4.42356653331032,-1.3907746702388,299.337738868711));
#9477=CARTESIAN_POINT('Ctrl Pts',(-1.27650149624862,-4.45788471095139,299.534155152271));
#9478=CARTESIAN_POINT('Ctrl Pts',(3.01699305348801,-3.52135574899054,299.730571435832));
#9479=CARTESIAN_POINT('Ctrl Pts',(4.600917373614,0.577713353443416,299.926987719392));
#9480=CARTESIAN_POINT('Ctrl Pts',(2.05274420541422,4.15793630930791,300.123404002952));
#9481=CARTESIAN_POINT('Ctrl Pts',(-2.33900455103209,4.00390446639706,300.319820286512));
#9482=CARTESIAN_POINT('Ctrl Pts',(-4.6300864471361,0.253954218616865,300.516236570073));
#9483=CARTESIAN_POINT('Ctrl Pts',(-2.76287407130117,-3.72407305174658,300.712652853633));
#9484=CARTESIAN_POINT('Ctrl Pts',(1.58568363771314,-4.35749935687765,300.909069137193));
#9485=CARTESIAN_POINT('Ctrl Pts',(4.51013420556256,-1.07744266171838,301.105485420753));
#9486=CARTESIAN_POINT('Ctrl Pts',(3.38401996759768,3.17026845839884,301.301901704314));
#9487=CARTESIAN_POINT('Ctrl Pts',(-0.781292563612361,4.57075214501524,301.498317987873));
#9488=CARTESIAN_POINT('Ctrl Pts',(-4.24492394387617,1.8662298763172,301.694734271434));
#9489=CARTESIAN_POINT('Ctrl Pts',(-3.89617663551077,-2.51435893727449,301.891150554994));
#9490=CARTESIAN_POINT('Ctrl Pts',(-0.0482616226496284,-4.63679458860285,
302.087566838554));
#9491=CARTESIAN_POINT('Ctrl Pts',(3.84299729542567,-2.5949113716598,302.283983122115));
#9492=CARTESIAN_POINT('Ctrl Pts',(4.28284903123359,1.77746938571041,302.480399405675));
#9493=CARTESIAN_POINT('Ctrl Pts',(0.876261445153081,4.55349965672981,302.676815689235));
#9494=CARTESIAN_POINT('Ctrl Pts',(-3.31729912253674,3.24001848146433,302.873231972795));
#9495=CARTESIAN_POINT('Ctrl Pts',(-4.53158358723572,-0.983332825142458,
303.069648256355));
#9496=CARTESIAN_POINT('Ctrl Pts',(-1.67603948710785,-4.32355003480224,303.266064539916));
#9497=CARTESIAN_POINT('Ctrl Pts',(2.68476059529826,-3.78077421582624,303.462480823476));
#9498=CARTESIAN_POINT('Ctrl Pts',(4.63436931529892,0.157526020028036,303.658897107036));
#9499=CARTESIAN_POINT('Ctrl Pts',(2.42183724715278,3.95435174763791,303.855313390597));
#9500=CARTESIAN_POINT('Ctrl Pts',(-1.96575384247124,4.19976237385744,304.051729674156));
#9501=CARTESIAN_POINT('Ctrl Pts',(-4.58789591526953,0.673354385635241,304.248145957717));
#9502=CARTESIAN_POINT('Ctrl Pts',(-3.08963453431999,-3.45779587166151,304.444562241277));
#9503=CARTESIAN_POINT('Ctrl Pts',(1.18343537924031,-4.48348796067515,304.640978524837));
#9504=CARTESIAN_POINT('Ctrl Pts',(4.39366134024968,-1.48254954638245,304.837394808398));
#9505=CARTESIAN_POINT('Ctrl Pts',(3.65792106471558,2.84987785549197,305.033811091958));
#9506=CARTESIAN_POINT('Ctrl Pts',(-0.3629960006453,4.62280693344557,305.230227375518));
#9507=CARTESIAN_POINT('Ctrl Pts',(-4.05793271056506,2.24401064282424,305.426643659078));
#9508=CARTESIAN_POINT('Ctrl Pts',(-4.10836974515988,-2.15020447963357,305.623059942638));
#9509=CARTESIAN_POINT('Ctrl Pts',(-0.469191989355248,-4.61317350694027,
305.819476226199));
#9510=CARTESIAN_POINT('Ctrl Pts',(3.59163297431157,-2.93333759691029,306.015892509759));
#9511=CARTESIAN_POINT('Ctrl Pts',(4.42624039881829,1.38157897222829,306.212308793319));
#9512=CARTESIAN_POINT('Ctrl Pts',(1.28683256078006,4.45435220162257,306.408725076879));
#9513=CARTESIAN_POINT('Ctrl Pts',(-3.0107876642197,3.52965939911648,306.60514136044));
#9514=CARTESIAN_POINT('Ctrl Pts',(-4.59869662196651,-0.570614468679802,
306.801557644));
#9515=CARTESIAN_POINT('Ctrl Pts',(-2.91065832330177,-2.94999883844826,306.93250183304));
#9516=CARTESIAN_POINT('Ctrl Pts',(-1.75025476627565,-3.5260053049299,306.99797392756));
#9517=CARTESIAN_POINT('Ctrl Pts',(-2.14477093771142,3.01083830192886,296.726262181086));
#9518=CARTESIAN_POINT('Ctrl Pts',(-3.13635843824042,2.30456100957975,296.791778926582));
#9519=CARTESIAN_POINT('Ctrl Pts',(-4.34934240402712,-0.153369226231343,
296.922767766599));
#9520=CARTESIAN_POINT('Ctrl Pts',(-2.26727971697993,-3.72017855073993,297.119228701135));
#9521=CARTESIAN_POINT('Ctrl Pts',(1.85502898798194,-3.9390476293032,297.315644984695));
#9522=CARTESIAN_POINT('Ctrl Pts',(4.30945449622017,-0.623400972107909,297.512061268256));
#9523=CARTESIAN_POINT('Ctrl Pts',(2.89446330738038,3.25354832817121,297.708477551816));
#9524=CARTESIAN_POINT('Ctrl Pts',(-1.12047912413229,4.20779803596913,297.904893835376));
#9525=CARTESIAN_POINT('Ctrl Pts',(-4.12891524017367,1.38332919810655,298.101310118936));
#9526=CARTESIAN_POINT('Ctrl Pts',(-3.42925459331503,-2.68366096823,298.297726402497));
#9527=CARTESIAN_POINT('Ctrl Pts',(0.350273968468058,-4.34037720151753,298.494142686057));
#9528=CARTESIAN_POINT('Ctrl Pts',(3.81519964975679,-2.09902084784856,298.690558969617));
#9529=CARTESIAN_POINT('Ctrl Pts',(3.85369306925529,2.02748779081302,298.886975253177));
#9530=CARTESIAN_POINT('Ctrl Pts',(0.431168807947103,4.33309640133782,299.083391536737));
#9531=CARTESIAN_POINT('Ctrl Pts',(-3.378587271054,2.74714179826662,299.279807820298));
#9532=CARTESIAN_POINT('Ctrl Pts',(-4.15402519123534,-1.3060305461667,299.476224103858));
#9533=CARTESIAN_POINT('Ctrl Pts',(-1.1987203836851,-4.18625225809752,299.672640387418));
#9534=CARTESIAN_POINT('Ctrl Pts',(2.83315850492985,-3.30678884977944,299.869056670978));
#9535=CARTESIAN_POINT('Ctrl Pts',(4.32056950627178,0.542511524455615,300.065472954539));
#9536=CARTESIAN_POINT('Ctrl Pts',(1.92766426733765,3.90458062343006,300.261889238099));
#9537=CARTESIAN_POINT('Ctrl Pts',(-2.19648190080015,3.75993440846169,300.458305521659));
#9538=CARTESIAN_POINT('Ctrl Pts',(-4.34796121956542,0.238480016884807,300.654721805219));
#9539=CARTESIAN_POINT('Ctrl Pts',(-2.59452376401972,-3.49715397167979,300.851138088779));
#9540=CARTESIAN_POINT('Ctrl Pts',(1.4890631183659,-4.09198368849123,301.047554372339));
#9541=CARTESIAN_POINT('Ctrl Pts',(4.23531803233416,-1.01179080843177,301.2439706559));
#9542=CARTESIAN_POINT('Ctrl Pts',(3.17782135459926,2.97709437396264,301.44038693946));
#9543=CARTESIAN_POINT('Ctrl Pts',(-0.733686035132803,4.29224233665535,301.63680322302));
#9544=CARTESIAN_POINT('Ctrl Pts',(-3.98626783726566,1.75251482270716,301.833219506581));
#9545=CARTESIAN_POINT('Ctrl Pts',(-3.6587707614522,-2.36115141178396,302.029635790141));
#9546=CARTESIAN_POINT('Ctrl Pts',(-0.0453208954238121,-4.35426061360174,
302.226052073701));
#9547=CARTESIAN_POINT('Ctrl Pts',(3.60883180005007,-2.43679554172575,302.422468357261));
#9548=CARTESIAN_POINT('Ctrl Pts',(4.02188203388193,1.66916277833516,302.618884640821));
#9549=CARTESIAN_POINT('Ctrl Pts',(0.822868174325886,4.27604109487238,302.815300924382));
#9550=CARTESIAN_POINT('Ctrl Pts',(-3.11516601324143,3.0425943163104,303.011717207942));
#9551=CARTESIAN_POINT('Ctrl Pts',(-4.25546043804587,-0.923415369985092,
303.208133491502));
#9552=CARTESIAN_POINT('Ctrl Pts',(-1.57391331147019,-4.06010300170498,303.404549775062));
#9553=CARTESIAN_POINT('Ctrl Pts',(2.52116997931962,-3.55040016164564,303.600966058622));
#9554=CARTESIAN_POINT('Ctrl Pts',(4.35198311956513,0.147927481262918,303.797382342183));
#9555=CARTESIAN_POINT('Ctrl Pts',(2.27426734920524,3.71340108733503,303.993798625743));
#9556=CARTESIAN_POINT('Ctrl Pts',(-1.8459744913755,3.9438580988519,304.190214909303));
#9557=CARTESIAN_POINT('Ctrl Pts',(-4.30834148492695,0.632324858119486,304.386631192864));
#9558=CARTESIAN_POINT('Ctrl Pts',(-2.9013737197418,-3.24710186879059,304.583047476424));
#9559=CARTESIAN_POINT('Ctrl Pts',(1.11132506780329,-4.21029542406532,304.779463759984));
#9560=CARTESIAN_POINT('Ctrl Pts',(4.12594221240204,-1.39221330041091,304.975880043544));
#9561=CARTESIAN_POINT('Ctrl Pts',(3.43503282610466,2.67622614343233,305.172296327104));
#9562=CARTESIAN_POINT('Ctrl Pts',(-0.340877552003241,4.34112526875001,305.368712610665));
#9563=CARTESIAN_POINT('Ctrl Pts',(-3.81067054764307,2.10727625989075,305.565128894225));
#9564=CARTESIAN_POINT('Ctrl Pts',(-3.8580343005561,-2.01918599108778,305.761545177785));
#9565=CARTESIAN_POINT('Ctrl Pts',(-0.440602696631977,-4.33207883617583,
305.957961461345));
#9566=CARTESIAN_POINT('Ctrl Pts',(3.37278387034834,-2.7546004293609,306.154377744905));
#9567=CARTESIAN_POINT('Ctrl Pts',(4.15653612999808,1.29739516996088,306.350794028466));
#9568=CARTESIAN_POINT('Ctrl Pts',(1.20842194508195,4.1829349952894,306.547210312026));
#9569=CARTESIAN_POINT('Ctrl Pts',(-2.8273312288738,3.31458653328722,306.743626595586));
#9570=CARTESIAN_POINT('Ctrl Pts',(-4.31848407176599,-0.535845196298082,
306.940042879146));
#9571=CARTESIAN_POINT('Ctrl Pts',(-2.73330307276428,-2.77024645085618,307.070987068187));
#9572=CARTESIAN_POINT('Ctrl Pts',(-1.64360642830614,-3.31115509415596,307.136459162707));
#9573=CARTESIAN_POINT('Ctrl Pts',(-2.00560364565601,2.81547468247249,296.864747416232));
#9574=CARTESIAN_POINT('Ctrl Pts',(-2.93285022060727,2.15502545338563,296.930264161729));
#9575=CARTESIAN_POINT('Ctrl Pts',(-4.06712755583635,-0.143417590127015,
297.061253001746));
#9576=CARTESIAN_POINT('Ctrl Pts',(-2.12016322402664,-3.478788122622,297.257713936283));
#9577=CARTESIAN_POINT('Ctrl Pts',(1.73466211970593,-3.68345549020403,297.454130219843));
#9578=CARTESIAN_POINT('Ctrl Pts',(4.0298278461524,-0.582950486870754,297.650546503403));
#9579=CARTESIAN_POINT('Ctrl Pts',(2.70665088724769,3.04243603527242,297.846962786964));
#9580=CARTESIAN_POINT('Ctrl Pts',(-1.04777483540462,3.93476754684532,298.043379070524));
#9581=CARTESIAN_POINT('Ctrl Pts',(-3.86100320211035,1.29356941297673,298.239795354084));
#9582=CARTESIAN_POINT('Ctrl Pts',(-3.20674128565643,-2.50952683428754,298.436211637644));
#9583=CARTESIAN_POINT('Ctrl Pts',(0.327545816565179,-4.05874407650011,298.632627921204));
#9584=CARTESIAN_POINT('Ctrl Pts',(3.56764360795687,-1.96282213206653,298.829044204765));
#9585=CARTESIAN_POINT('Ctrl Pts',(3.60363931319628,1.89593062516814,299.025460488325));
#9586=CARTESIAN_POINT('Ctrl Pts',(0.403191649936562,4.05193570404087,299.221876771885));
#9587=CARTESIAN_POINT('Ctrl Pts',(-3.15936160307328,2.56888859731411,299.418293055445));
#9588=CARTESIAN_POINT('Ctrl Pts',(-3.88448384916037,-1.2212864220946,299.614709339006));
#9589=CARTESIAN_POINT('Ctrl Pts',(-1.12093927112159,-3.91461980524366,299.811125622566));
#9590=CARTESIAN_POINT('Ctrl Pts',(2.64932395637171,-3.09222195056834,300.007541906126));
#9591=CARTESIAN_POINT('Ctrl Pts',(4.04022163892955,0.507309695467813,300.203958189686));
#9592=CARTESIAN_POINT('Ctrl Pts',(1.80258432926109,3.65122493755221,300.400374473246));
#9593=CARTESIAN_POINT('Ctrl Pts',(-2.05395925056823,3.51596435052632,300.596790756806));
#9594=CARTESIAN_POINT('Ctrl Pts',(-4.06583599199474,0.223005815152753,300.793207040367));
#9595=CARTESIAN_POINT('Ctrl Pts',(-2.42617345673829,-3.270234891613,300.989623323927));
#9596=CARTESIAN_POINT('Ctrl Pts',(1.39244259901866,-3.82646802010482,301.186039607487));
#9597=CARTESIAN_POINT('Ctrl Pts',(3.96050185910575,-0.946138955145171,301.382455891047));
#9598=CARTESIAN_POINT('Ctrl Pts',(2.97162274160084,2.78392028952646,301.578872174608));
#9599=CARTESIAN_POINT('Ctrl Pts',(-0.686079506653246,4.01373252829545,301.775288458168));
#9600=CARTESIAN_POINT('Ctrl Pts',(-3.72761173065515,1.63879976909712,301.971704741728));
#9601=CARTESIAN_POINT('Ctrl Pts',(-3.42136488739364,-2.20794388629344,302.168121025288));
#9602=CARTESIAN_POINT('Ctrl Pts',(-0.0423801681979951,-4.07172663860065,
302.364537308849));
#9603=CARTESIAN_POINT('Ctrl Pts',(3.37466630467447,-2.27867971179171,302.560953592409));
#9604=CARTESIAN_POINT('Ctrl Pts',(3.76091503653028,1.56085617095991,302.757369875969));
#9605=CARTESIAN_POINT('Ctrl Pts',(0.769474903498698,3.99858253301496,302.953786159529));
#9606=CARTESIAN_POINT('Ctrl Pts',(-2.91303290394612,2.84517015115646,303.150202443089));
#9607=CARTESIAN_POINT('Ctrl Pts',(-3.97933728885602,-0.86349791482772,303.34661872665));
#9608=CARTESIAN_POINT('Ctrl Pts',(-1.47178713583252,-3.79665596860773,303.54303501021));
#9609=CARTESIAN_POINT('Ctrl Pts',(2.35757936334099,-3.32002610746504,303.73945129377));
#9610=CARTESIAN_POINT('Ctrl Pts',(4.06959692383135,0.138328942497795,303.93586757733));
#9611=CARTESIAN_POINT('Ctrl Pts',(2.1266974512577,3.47245042703215,304.132283860891));
#9612=CARTESIAN_POINT('Ctrl Pts',(-1.72619514027976,3.68795382384636,304.328700144451));
#9613=CARTESIAN_POINT('Ctrl Pts',(-4.02878705458437,0.591295330603737,304.525116428011));
#9614=CARTESIAN_POINT('Ctrl Pts',(-2.7131129051636,-3.03640786591968,304.721532711571));
#9615=CARTESIAN_POINT('Ctrl Pts',(1.03921475636626,-3.93710288745548,304.917948995132));
#9616=CARTESIAN_POINT('Ctrl Pts',(3.8582230845544,-1.30187705443938,305.114365278692));
#9617=CARTESIAN_POINT('Ctrl Pts',(3.21214458749373,2.50257443137269,305.310781562252));
#9618=CARTESIAN_POINT('Ctrl Pts',(-0.318759103361179,4.05944360405444,305.507197845812));
#9619=CARTESIAN_POINT('Ctrl Pts',(-3.56340838472108,1.97054187695727,305.703614129372));
#9620=CARTESIAN_POINT('Ctrl Pts',(-3.60769885595232,-1.888167502542,305.900030412933));
#9621=CARTESIAN_POINT('Ctrl Pts',(-0.412013403908709,-4.05098416541141,
306.096446696493));
#9622=CARTESIAN_POINT('Ctrl Pts',(3.15393476638512,-2.57586326181149,306.292862980053));
#9623=CARTESIAN_POINT('Ctrl Pts',(3.88683186117788,1.21321136769346,306.489279263613));
#9624=CARTESIAN_POINT('Ctrl Pts',(1.13001132938383,3.91151778895623,306.685695547173));
#9625=CARTESIAN_POINT('Ctrl Pts',(-2.6438747935279,3.09951366745796,306.882111830734));
#9626=CARTESIAN_POINT('Ctrl Pts',(-4.03827152156548,-0.50107592391636,307.078528114294));
#9627=CARTESIAN_POINT('Ctrl Pts',(-2.5559478222268,-2.5904940632641,307.209472303334));
#9628=CARTESIAN_POINT('Ctrl Pts',(-1.53695809033663,-3.09630488338201,307.274944397854));
#9629=CARTESIAN_POINT('Ctrl Pts',(-1.86643635360062,2.62011106301612,297.00323265138));
#9630=CARTESIAN_POINT('Ctrl Pts',(-2.72934200297413,2.00548989719149,297.068749396876));
#9631=CARTESIAN_POINT('Ctrl Pts',(-3.7849127076456,-0.13346595402269,297.199738236893));
#9632=CARTESIAN_POINT('Ctrl Pts',(-1.97304673107334,-3.23739769450407,297.396199171429));
#9633=CARTESIAN_POINT('Ctrl Pts',(1.61429525142993,-3.42786335110486,297.59261545499));
#9634=CARTESIAN_POINT('Ctrl Pts',(3.75020119608464,-0.542500001633599,297.78903173855));
#9635=CARTESIAN_POINT('Ctrl Pts',(2.51883846711499,2.83132374237361,297.98544802211));
#9636=CARTESIAN_POINT('Ctrl Pts',(-0.97507054667695,3.66173705772152,298.18186430567));
#9637=CARTESIAN_POINT('Ctrl Pts',(-3.59309116404703,1.20380962784691,298.378280589231));
#9638=CARTESIAN_POINT('Ctrl Pts',(-2.98422797799783,-2.33539270034508,298.574696872791));
#9639=CARTESIAN_POINT('Ctrl Pts',(0.304817664662298,-3.7771109514827,298.771113156351));
#9640=CARTESIAN_POINT('Ctrl Pts',(3.32008756615693,-1.82662341628449,298.967529439911));
#9641=CARTESIAN_POINT('Ctrl Pts',(3.35358555713727,1.76437345952326,299.163945723471));
#9642=CARTESIAN_POINT('Ctrl Pts',(0.375214491926022,3.77077500674391,299.360362007032));
#9643=CARTESIAN_POINT('Ctrl Pts',(-2.94013593509256,2.39063539636159,299.556778290592));
#9644=CARTESIAN_POINT('Ctrl Pts',(-3.61494250708539,-1.13654229802251,299.753194574152));
#9645=CARTESIAN_POINT('Ctrl Pts',(-1.04315815855808,-3.64298735238979,299.949610857712));
#9646=CARTESIAN_POINT('Ctrl Pts',(2.46548940781356,-2.87765505135725,300.146027141273));
#9647=CARTESIAN_POINT('Ctrl Pts',(3.75987377158732,0.472107866480012,300.342443424833));
#9648=CARTESIAN_POINT('Ctrl Pts',(1.67750439118453,3.39786925167437,300.538859708393));
#9649=CARTESIAN_POINT('Ctrl Pts',(-1.9114366003363,3.27199429259095,300.735275991953));
#9650=CARTESIAN_POINT('Ctrl Pts',(-3.78371076442406,0.207531613420697,300.931692275514));
#9651=CARTESIAN_POINT('Ctrl Pts',(-2.25782314945684,-3.04331581154621,301.128108559074));
#9652=CARTESIAN_POINT('Ctrl Pts',(1.29582207967142,-3.5609523517184,301.324524842634));
#9653=CARTESIAN_POINT('Ctrl Pts',(3.68568568587734,-0.880487101858563,301.520941126194));
#9654=CARTESIAN_POINT('Ctrl Pts',(2.76542412860242,2.59074620509027,301.717357409755));
#9655=CARTESIAN_POINT('Ctrl Pts',(-0.638472978173689,3.73522271993555,301.913773693315));
#9656=CARTESIAN_POINT('Ctrl Pts',(-3.46895562404465,1.52508471548708,302.110189976875));
#9657=CARTESIAN_POINT('Ctrl Pts',(-3.18395901333507,-2.05473636080292,302.306606260435));
#9658=CARTESIAN_POINT('Ctrl Pts',(-0.0394394409721774,-3.78919266359954,
302.503022543995));
#9659=CARTESIAN_POINT('Ctrl Pts',(3.14050080929887,-2.12056388185767,302.699438827556));
#9660=CARTESIAN_POINT('Ctrl Pts',(3.49994803917864,1.45254956358465,302.895855111116));
#9661=CARTESIAN_POINT('Ctrl Pts',(0.716081632671503,3.72112397115754,303.092271394676));
#9662=CARTESIAN_POINT('Ctrl Pts',(-2.71089979465081,2.64774598600254,303.288687678236));
#9663=CARTESIAN_POINT('Ctrl Pts',(-3.70321413966617,-0.803580459670354,
303.485103961796));
#9664=CARTESIAN_POINT('Ctrl Pts',(-1.36966096019486,-3.53320893551047,303.681520245357));
#9665=CARTESIAN_POINT('Ctrl Pts',(2.19398874736236,-3.08965205328445,303.877936528917));
#9666=CARTESIAN_POINT('Ctrl Pts',(3.78721072809757,0.128730403732677,304.074352812477));
#9667=CARTESIAN_POINT('Ctrl Pts',(1.97912755331017,3.23149976672927,304.270769096037));
#9668=CARTESIAN_POINT('Ctrl Pts',(-1.60641578918403,3.43204954884082,304.467185379597));
#9669=CARTESIAN_POINT('Ctrl Pts',(-3.74923262424179,0.550265803087981,304.663601663158));
#9670=CARTESIAN_POINT('Ctrl Pts',(-2.52485209058541,-2.82571386304877,304.860017946718));
#9671=CARTESIAN_POINT('Ctrl Pts',(0.967104444929231,-3.66391035084566,305.056434230278));
#9672=CARTESIAN_POINT('Ctrl Pts',(3.59050395670676,-1.21154080846783,305.252850513839));
#9673=CARTESIAN_POINT('Ctrl Pts',(2.98925634888281,2.32892271931305,305.449266797398));
#9674=CARTESIAN_POINT('Ctrl Pts',(-0.29664065471912,3.77776193935887,305.645683080959));
#9675=CARTESIAN_POINT('Ctrl Pts',(-3.31614622179908,1.83380749402379,305.842099364519));
#9676=CARTESIAN_POINT('Ctrl Pts',(-3.35736341134853,-1.75714901399621,306.038515648079));
#9677=CARTESIAN_POINT('Ctrl Pts',(-0.383424111185439,-3.76988949464697,
306.23493193164));
#9678=CARTESIAN_POINT('Ctrl Pts',(2.93508566242189,-2.39712609426209,306.4313482152));
#9679=CARTESIAN_POINT('Ctrl Pts',(3.61712759235767,1.12902756542604,306.62776449876));
#9680=CARTESIAN_POINT('Ctrl Pts',(1.05160071368571,3.64010058262307,306.82418078232));
#9681=CARTESIAN_POINT('Ctrl Pts',(-2.460418358182,2.88444080162871,307.02059706588));
#9682=CARTESIAN_POINT('Ctrl Pts',(-3.75805897136496,-0.466306651534639,
307.217013349441));
#9683=CARTESIAN_POINT('Ctrl Pts',(-2.37859257168932,-2.41074167567201,307.347957538481));
#9684=CARTESIAN_POINT('Ctrl Pts',(-1.43030975236712,-2.88145467260807,307.413429633001));
#9685=CARTESIAN_POINT('',(-1.8740725398893,2.62480419192483,307.001415228007));
#9686=CARTESIAN_POINT('Ctrl Pts',(-1.87562241821632,2.62673369148108,307.));
#9687=CARTESIAN_POINT('Ctrl Pts',(-1.95770449094995,2.58115596232075,307.));
#9688=CARTESIAN_POINT('Ctrl Pts',(-2.03743863910024,2.53192586541867,307.));
#9689=CARTESIAN_POINT('Ctrl Pts',(-2.11454810906558,2.47911769610372,307.));
#9690=CARTESIAN_POINT('Ctrl Pts',(-2.19910585323819,2.42120860046132,307.));
#9691=CARTESIAN_POINT('Ctrl Pts',(-2.28050877294379,2.35899810945558,307.));
#9692=CARTESIAN_POINT('Ctrl Pts',(-2.35867943255216,2.29288564826134,307.));
#9693=CARTESIAN_POINT('Ctrl Pts',(-2.43922435958225,2.22476516175978,307.));
#9694=CARTESIAN_POINT('Ctrl Pts',(-2.51633824355233,2.1525017186583,307.));
#9695=CARTESIAN_POINT('Ctrl Pts',(-2.58991395366746,2.07648048712394,307.));
#9696=CARTESIAN_POINT('Ctrl Pts',(-2.66337435931201,2.00057839256892,307.));
#9697=CARTESIAN_POINT('Ctrl Pts',(-2.7333081306884,1.92092961365071,307.));
#9698=CARTESIAN_POINT('Ctrl Pts',(-2.79957919033415,1.83787484209342,307.));
#9699=CARTESIAN_POINT('Ctrl Pts',(-2.80893754976685,1.82614639819968,307.));
#9700=CARTESIAN_POINT('Ctrl Pts',(-2.81822281557543,1.8143499747194,307.));
#9701=CARTESIAN_POINT('Ctrl Pts',(-2.82743454884594,1.80248647431831,307.));
#9702=CARTESIAN_POINT('Ctrl Pts',(-2.83706693497037,1.79008122838958,307.));
#9703=CARTESIAN_POINT('Ctrl Pts',(-2.84661330232596,1.7776098546387,307.));
#9704=CARTESIAN_POINT('Ctrl Pts',(-2.85607185997111,1.76507574247541,307.));
#9705=CARTESIAN_POINT('Ctrl Pts',(-2.92166160942224,1.67815876134315,307.));
#9706=CARTESIAN_POINT('Ctrl Pts',(-2.98305537122714,1.58819739798644,307.));
#9707=CARTESIAN_POINT('Ctrl Pts',(-3.04016414393303,1.49562175005816,307.));
#9708=CARTESIAN_POINT('Ctrl Pts',(-3.09822312230499,1.40150578002114,307.));
#9709=CARTESIAN_POINT('Ctrl Pts',(-3.15185387969084,1.30468720717543,307.));
#9710=CARTESIAN_POINT('Ctrl Pts',(-3.20093354890556,1.20557190624194,307.));
#9711=CARTESIAN_POINT('Ctrl Pts',(-3.25050203129707,1.10546945796429,307.));
#9712=CARTESIAN_POINT('Ctrl Pts',(-3.29542889000202,1.00302358346718,307.));
#9713=CARTESIAN_POINT('Ctrl Pts',(-3.3355494236701,0.898615931380555,307.));
#9714=CARTESIAN_POINT('Ctrl Pts',(-3.35616396299268,0.844969694585103,307.));
#9715=CARTESIAN_POINT('Ctrl Pts',(-3.37550893595618,0.790805015894116,307.));
#9716=CARTESIAN_POINT('Ctrl Pts',(-3.39355738158136,0.736170952424262,307.));
#9717=CARTESIAN_POINT('Ctrl Pts',(-3.40458316148461,0.702795050058588,307.));
#9718=CARTESIAN_POINT('Ctrl Pts',(-3.41512501640732,0.669243942651207,307.));
#9719=CARTESIAN_POINT('Ctrl Pts',(-3.42517616166359,0.635528570480346,307.));
#9720=CARTESIAN_POINT('Ctrl Pts',(-3.4296359472032,0.62056874993885,307.));
#9721=CARTESIAN_POINT('Ctrl Pts',(-3.43399864147103,0.605577994095616,307.));
#9722=CARTESIAN_POINT('Ctrl Pts',(-3.43826050148757,0.59056902651178,307.));
#9723=CARTESIAN_POINT('Ctrl Pts',(-3.46965055336494,0.480022863743607,307.));
#9724=CARTESIAN_POINT('Ctrl Pts',(-3.49562521356327,0.368320523725974,307.));
#9725=CARTESIAN_POINT('Ctrl Pts',(-3.51606074258901,0.255892602399452,307.));
#9726=CARTESIAN_POINT('Ctrl Pts',(-3.53696881357864,0.140864948485883,307.));
#9727=CARTESIAN_POINT('Ctrl Pts',(-3.55207933732713,0.0250769828317131,
307.));
#9728=CARTESIAN_POINT('Ctrl Pts',(-3.56121413083353,-0.0910426031961557,
307.));
#9729=CARTESIAN_POINT('Ctrl Pts',(-3.57034892433994,-0.207162189224066,
307.));
#9730=CARTESIAN_POINT('Ctrl Pts',(-3.57350856690181,-0.323614351558602,
307.));
#9731=CARTESIAN_POINT('Ctrl Pts',(-3.57046020776024,-0.439989127307766,
307.));
#9732=CARTESIAN_POINT('Ctrl Pts',(-3.56844092581946,-0.51707764349632,307.));
#9733=CARTESIAN_POINT('Ctrl Pts',(-3.56369641416304,-0.594132558068256,
307.));
#9734=CARTESIAN_POINT('Ctrl Pts',(-3.5562979507555,-0.671059667724272,307.));
#9735=CARTESIAN_POINT('Ctrl Pts',(-3.55447014995795,-0.690064618433204,
307.));
#9736=CARTESIAN_POINT('Ctrl Pts',(-3.55248030988035,-0.70906176810033,307.));
#9737=CARTESIAN_POINT('Ctrl Pts',(-3.55032939438232,-0.72804969199813,307.));
#9738=CARTESIAN_POINT('Ctrl Pts',(-3.54825093279214,-0.746398004860717,
307.));
#9739=CARTESIAN_POINT('Ctrl Pts',(-3.54602283507798,-0.764730434923112,
307.));
#9740=CARTESIAN_POINT('Ctrl Pts',(-3.54364770171127,-0.78303604758736,307.));
#9741=CARTESIAN_POINT('Ctrl Pts',(-3.52915857158688,-0.894706578436623,
307.));
#9742=CARTESIAN_POINT('Ctrl Pts',(-3.50918968560073,-1.00548797552805,307.));
#9743=CARTESIAN_POINT('Ctrl Pts',(-3.48405567932025,-1.11508513485562,307.));
#9744=CARTESIAN_POINT('Ctrl Pts',(-3.45845720380376,-1.22670761829162,307.));
#9745=CARTESIAN_POINT('Ctrl Pts',(-3.42750082039565,-1.33710233523251,307.));
#9746=CARTESIAN_POINT('Ctrl Pts',(-3.39146415702186,-1.44596592372902,307.));
#9747=CARTESIAN_POINT('Ctrl Pts',(-3.3547045784688,-1.55701337535897,307.));
#9748=CARTESIAN_POINT('Ctrl Pts',(-3.31265870899318,-1.66646840900814,307.));
#9749=CARTESIAN_POINT('Ctrl Pts',(-3.26556674632985,-1.77400697166853,307.));
#9750=CARTESIAN_POINT('Ctrl Pts',(-3.22694700310801,-1.86219848974312,307.));
#9751=CARTESIAN_POINT('Ctrl Pts',(-3.18493241340503,-1.94910124535555,307.));
#9752=CARTESIAN_POINT('Ctrl Pts',(-3.13963017239118,-2.03452991644561,307.));
#9753=CARTESIAN_POINT('Ctrl Pts',(-3.13126875800696,-2.05029744810168,307.));
#9754=CARTESIAN_POINT('Ctrl Pts',(-3.12279528754488,-2.06601473950236,307.));
#9755=CARTESIAN_POINT('Ctrl Pts',(-3.11421035577053,-2.08168058964027,307.));
#9756=CARTESIAN_POINT('Ctrl Pts',(-3.10572159975257,-2.09717093751141,307.));
#9757=CARTESIAN_POINT('Ctrl Pts',(-3.09712808038243,-2.11260327499777,307.));
#9758=CARTESIAN_POINT('Ctrl Pts',(-3.08843198120147,-2.12797434134853,307.));
#9759=CARTESIAN_POINT('Ctrl Pts',(-3.02913621757971,-2.23278445194894,307.));
#9760=CARTESIAN_POINT('Ctrl Pts',(-2.96505698426078,-2.33477997371097,307.));
#9761=CARTESIAN_POINT('Ctrl Pts',(-2.8964711255631,-2.43362682562493,307.));
#9762=CARTESIAN_POINT('Ctrl Pts',(-2.82741050084661,-2.53315791664076,307.));
#9763=CARTESIAN_POINT('Ctrl Pts',(-2.75378032677603,-2.62949742827724,307.));
#9764=CARTESIAN_POINT('Ctrl Pts',(-2.67581266947912,-2.72228997936985,307.));
#9765=CARTESIAN_POINT('Ctrl Pts',(-2.6409583266364,-2.76377158214157,307.));
#9766=CARTESIAN_POINT('Ctrl Pts',(-2.60523653444311,-2.80454409027921,307.));
#9767=CARTESIAN_POINT('Ctrl Pts',(-2.56866505040167,-2.84457415493151,307.));
#9768=CARTESIAN_POINT('Ctrl Pts',(-2.54450137491384,-2.87102299936229,307.));
#9769=CARTESIAN_POINT('Ctrl Pts',(-2.51996073222418,-2.89715358568975,307.));
#9770=CARTESIAN_POINT('Ctrl Pts',(-2.49508271396498,-2.92292083144206,307.));
#9771=CARTESIAN_POINT('Ctrl Pts',(-2.40941490538101,-3.01165070750563,307.));
#9772=CARTESIAN_POINT('Ctrl Pts',(-2.31968801564158,-3.09614586137004,307.));
#9773=CARTESIAN_POINT('Ctrl Pts',(-2.22615742676719,-3.17605066264026,307.));
#9774=CARTESIAN_POINT('Ctrl Pts',(-2.13385009249119,-3.25491041633018,307.));
#9775=CARTESIAN_POINT('Ctrl Pts',(-2.03783742037138,-3.32929985577124,307.));
#9776=CARTESIAN_POINT('Ctrl Pts',(-1.93832242401188,-3.39885060197879,307.));
#9777=CARTESIAN_POINT('Ctrl Pts',(-1.87645376288492,-3.44209043221199,307.));
#9778=CARTESIAN_POINT('Ctrl Pts',(-1.81323059511134,-3.48345947870024,307.));
#9779=CARTESIAN_POINT('Ctrl Pts',(-1.74869447533109,-3.52286199445089,307.));
#9780=CARTESIAN_POINT('Ctrl Pts',(-1.83773660687461,2.64742171296018,307.));
#9781=CARTESIAN_POINT('Ctrl Pts',(-1.84943329741252,2.63930232787106,307.000471742669));
#9782=CARTESIAN_POINT('Ctrl Pts',(-1.86107617823706,2.63110542515543,307.000943485338));
#9783=CARTESIAN_POINT('Ctrl Pts',(-1.87266422666468,2.62283172481011,307.001415228007));
#9784=CARTESIAN_POINT('Origin',(0.,0.,307.));
#9785=CARTESIAN_POINT('Origin',(0.,0.,177.));
#9786=CARTESIAN_POINT('',(0.,0.,0.));
#9787=CARTESIAN_POINT('Origin',(-33.8518529101985,-1.5,308.5));
#9788=CARTESIAN_POINT('',(-40.3518529101985,-1.5,307.));
#9789=CARTESIAN_POINT('',(-33.8518529101985,-8.,307.));
#9790=CARTESIAN_POINT('Origin',(-33.8518529101985,-1.5,307.));
#9791=CARTESIAN_POINT('',(-33.8518529101985,-8.,309.));
#9792=CARTESIAN_POINT('',(-33.8518529101985,-8.,308.5));
#9793=CARTESIAN_POINT('',(-40.3518529101985,-1.5,309.));
#9794=CARTESIAN_POINT('Origin',(-33.8518529101985,-1.5,309.));
#9795=CARTESIAN_POINT('',(-40.3518529101985,-1.5,308.5));
#9796=CARTESIAN_POINT('Origin',(-40.3518529101985,0.,307.));
#9797=CARTESIAN_POINT('',(-40.3518529101985,1.5,307.));
#9798=CARTESIAN_POINT('',(-40.3518529101985,0.,307.));
#9799=CARTESIAN_POINT('',(-33.8518529101985,8.,307.));
#9800=CARTESIAN_POINT('Origin',(-33.8518529101985,1.5,307.));
#9801=CARTESIAN_POINT('',(19.6481470898015,8.,307.));
#9802=CARTESIAN_POINT('',(19.6481470898015,8.,307.));
#9803=CARTESIAN_POINT('',(19.6481470898015,-8.,307.));
#9804=CARTESIAN_POINT('',(19.6481470898015,0.,307.));
#9805=CARTESIAN_POINT('',(19.6481470898015,-8.,307.));
#9806=CARTESIAN_POINT('Origin',(-33.8518529101985,1.5,308.5));
#9807=CARTESIAN_POINT('',(-40.3518529101985,1.5,309.));
#9808=CARTESIAN_POINT('',(-40.3518529101985,1.5,308.5));
#9809=CARTESIAN_POINT('',(-33.8518529101985,8.,309.));
#9810=CARTESIAN_POINT('Origin',(-33.8518529101985,1.5,309.));
#9811=CARTESIAN_POINT('',(-33.8518529101985,8.,308.5));
#9812=CARTESIAN_POINT('Origin',(-40.3518529101985,0.,309.));
#9813=CARTESIAN_POINT('',(-40.3518529101985,0.,309.));
#9814=CARTESIAN_POINT('Origin',(19.6481470898015,0.,309.));
#9815=CARTESIAN_POINT('',(-20.0405545273386,6.,309.));
#9816=CARTESIAN_POINT('',(-20.0405545273386,8.,309.));
#9817=CARTESIAN_POINT('',(-20.0405545273386,-8.,309.));
#9818=CARTESIAN_POINT('',(-40.3518529101985,8.,309.));
#9819=CARTESIAN_POINT('',(-20.0405545273386,-8.,309.));
#9820=CARTESIAN_POINT('',(-40.3518529101985,-8.,309.));
#9821=CARTESIAN_POINT('',(-20.0405545273386,-6.,309.));
#9822=CARTESIAN_POINT('',(-20.0405545273386,-8.,309.));
#9823=CARTESIAN_POINT('',(16.317900533139,-6.,309.));
#9824=CARTESIAN_POINT('',(-40.3518529101985,-6.,309.));
#9825=CARTESIAN_POINT('',(16.317900533139,-8.,309.));
#9826=CARTESIAN_POINT('',(16.317900533139,-8.,309.));
#9827=CARTESIAN_POINT('',(19.6481470898015,-8.,309.));
#9828=CARTESIAN_POINT('',(-40.3518529101985,-8.,309.));
#9829=CARTESIAN_POINT('',(19.6481470898015,8.,309.));
#9830=CARTESIAN_POINT('',(19.6481470898015,0.,309.));
#9831=CARTESIAN_POINT('',(16.317900533139,8.,309.));
#9832=CARTESIAN_POINT('',(-40.3518529101985,8.,309.));
#9833=CARTESIAN_POINT('',(16.317900533139,6.,309.));
#9834=CARTESIAN_POINT('',(16.317900533139,-8.,309.));
#9835=CARTESIAN_POINT('',(-40.3518529101985,6.,309.));
#9836=CARTESIAN_POINT('Origin',(19.6481470898015,0.,307.));
#9837=CARTESIAN_POINT('',(19.6481470898015,-8.,309.));
#9838=CARTESIAN_POINT('',(19.6481470898015,8.,309.));
#9839=CARTESIAN_POINT('Origin',(-16.022313954939,1.83573964553602,309.));
#9840=CARTESIAN_POINT('',(-16.022313954939,1.83573964553602,315.598323807971));
#9841=CARTESIAN_POINT('',(-34.7643786318829,1.83573964553602,326.55931644625));
#9842=CARTESIAN_POINT('Ctrl Pts',(-16.0223139548895,1.83573964553602,315.598323807965));
#9843=CARTESIAN_POINT('Ctrl Pts',(-16.6152689891987,1.83573964553602,315.668297772475));
#9844=CARTESIAN_POINT('Ctrl Pts',(-17.2033333974167,1.83573964553602,315.740204222438));
#9845=CARTESIAN_POINT('Ctrl Pts',(-17.7851093363551,1.83573964553602,315.814088969387));
#9846=CARTESIAN_POINT('Ctrl Pts',(-18.4542017359588,1.83573964553602,315.899062787177));
#9847=CARTESIAN_POINT('Ctrl Pts',(-19.1149750768524,1.83573964553602,315.986652476638));
#9848=CARTESIAN_POINT('Ctrl Pts',(-19.7652319532494,1.83573964553602,316.076948464976));
#9849=CARTESIAN_POINT('Ctrl Pts',(-20.4968760662518,1.83573964553602,316.178546050013));
#9850=CARTESIAN_POINT('Ctrl Pts',(-21.2152020044943,1.83573964553602,316.283568335362));
#9851=CARTESIAN_POINT('Ctrl Pts',(-21.9170421525721,1.83573964553602,316.392187427951));
#9852=CARTESIAN_POINT('Ctrl Pts',(-22.4830261868681,1.83573964553602,316.479780980975));
#9853=CARTESIAN_POINT('Ctrl Pts',(-23.0382867152506,1.83573964553602,316.569714291766));
#9854=CARTESIAN_POINT('Ctrl Pts',(-23.5811846866938,1.83573964553602,316.662104539026));
#9855=CARTESIAN_POINT('Ctrl Pts',(-24.0619814687136,1.83573964553602,316.743926420685));
#9856=CARTESIAN_POINT('Ctrl Pts',(-24.5330814352488,1.83573964553602,316.827675498925));
#9857=CARTESIAN_POINT('Ctrl Pts',(-24.9933830518898,1.83573964553602,316.913452048499));
#9858=CARTESIAN_POINT('Ctrl Pts',(-25.4232276652359,1.83573964553602,316.993552978959));
#9859=CARTESIAN_POINT('Ctrl Pts',(-25.8436552271082,1.83573964553602,317.07542204276));
#9860=CARTESIAN_POINT('Ctrl Pts',(-26.2538110895873,1.83573964553602,317.159156712438));
#9861=CARTESIAN_POINT('Ctrl Pts',(-26.6441668564352,1.83573964553602,317.238849127405));
#9862=CARTESIAN_POINT('Ctrl Pts',(-27.0252184159128,1.83573964553602,317.320231429346));
#9863=CARTESIAN_POINT('Ctrl Pts',(-27.3962737071739,1.83573964553602,317.403401459965));
#9864=CARTESIAN_POINT('Ctrl Pts',(-27.7503453005567,1.83573964553602,317.482764686839));
#9865=CARTESIAN_POINT('Ctrl Pts',(-28.0953145640723,1.83573964553602,317.563755774749));
#9866=CARTESIAN_POINT('Ctrl Pts',(-28.4306252622026,1.83573964553602,317.646471925112));
#9867=CARTESIAN_POINT('Ctrl Pts',(-28.7501141835393,1.83573964553602,317.725285079014));
#9868=CARTESIAN_POINT('Ctrl Pts',(-29.0608342542028,1.83573964553602,317.805664336882));
#9869=CARTESIAN_POINT('Ctrl Pts',(-29.3623498110856,1.83573964553602,317.887704925849));
#9870=CARTESIAN_POINT('Ctrl Pts',(-29.6523265222377,1.83573964553602,317.96660586355));
#9871=CARTESIAN_POINT('Ctrl Pts',(-29.9337895272155,1.83573964553602,318.047043401166));
#9872=CARTESIAN_POINT('Ctrl Pts',(-30.2063979120281,1.83573964553602,318.12911291368));
#9873=CARTESIAN_POINT('Ctrl Pts',(-30.4741983207634,1.83573964553602,318.209734971622));
#9874=CARTESIAN_POINT('Ctrl Pts',(-30.733453478094,1.83573964553602,318.291931941205));
#9875=CARTESIAN_POINT('Ctrl Pts',(-30.9838897802548,1.83573964553602,318.375804995173));
#9876=CARTESIAN_POINT('Ctrl Pts',(-31.235085850916,1.83573964553602,318.459932501487));
#9877=CARTESIAN_POINT('Ctrl Pts',(-31.4774094804883,1.83573964553602,318.545746357418));
#9878=CARTESIAN_POINT('Ctrl Pts',(-31.7106360658033,1.83573964553602,318.633358865222));
#9879=CARTESIAN_POINT('Ctrl Pts',(-31.9446281429948,1.83573964553602,318.721258933138));
#9880=CARTESIAN_POINT('Ctrl Pts',(-32.1694633663929,1.83573964553602,318.810969561697));
#9881=CARTESIAN_POINT('Ctrl Pts',(-32.3849665985943,1.83573964553602,318.902613194341));
#9882=CARTESIAN_POINT('Ctrl Pts',(-32.6034685743786,1.83573964553602,318.995532054982));
#9883=CARTESIAN_POINT('Ctrl Pts',(-32.8123770460666,1.83573964553602,319.090438190617));
#9884=CARTESIAN_POINT('Ctrl Pts',(-33.0115629265537,1.83573964553602,319.187467234392));
#9885=CARTESIAN_POINT('Ctrl Pts',(-33.2245143369608,1.83573964553602,319.291201854897));
#9886=CARTESIAN_POINT('Ctrl Pts',(-33.4263528949916,1.83573964553602,319.397363178007));
#9887=CARTESIAN_POINT('Ctrl Pts',(-33.6169817448998,1.83573964553602,319.506123424921));
#9888=CARTESIAN_POINT('Ctrl Pts',(-33.8180636092573,1.83573964553602,319.620847472347));
#9889=CARTESIAN_POINT('Ctrl Pts',(-34.0066730565997,1.83573964553602,319.738463663551));
#9890=CARTESIAN_POINT('Ctrl Pts',(-34.1827589496644,1.83573964553602,319.859176194319));
#9891=CARTESIAN_POINT('Ctrl Pts',(-34.3681788381234,1.83573964553602,319.986287478482));
#9892=CARTESIAN_POINT('Ctrl Pts',(-34.5397127794776,1.83573964553602,320.116832623688));
#9893=CARTESIAN_POINT('Ctrl Pts',(-34.6973613341441,1.83573964553602,320.251044787742));
#9894=CARTESIAN_POINT('Ctrl Pts',(-34.8627482473033,1.83573964553602,320.391844908417));
#9895=CARTESIAN_POINT('Ctrl Pts',(-35.0128537576466,1.83573964553602,320.536681652576));
#9896=CARTESIAN_POINT('Ctrl Pts',(-35.1477349540007,1.83573964553602,320.685808129403));
#9897=CARTESIAN_POINT('Ctrl Pts',(-35.2876536117633,1.83573964553602,320.840504091765));
#9898=CARTESIAN_POINT('Ctrl Pts',(-35.4111905301923,1.83573964553602,320.999817147191));
#9899=CARTESIAN_POINT('Ctrl Pts',(-35.5184561722676,1.83573964553602,321.163999379985));
#9900=CARTESIAN_POINT('Ctrl Pts',(-35.6268225696939,1.83573964553602,321.329866443708));
#9901=CARTESIAN_POINT('Ctrl Pts',(-35.7185833239258,1.83573964553602,321.500703866045));
#9902=CARTESIAN_POINT('Ctrl Pts',(-35.7938813306046,1.83573964553602,321.676728264262));
#9903=CARTESIAN_POINT('Ctrl Pts',(-35.8676199592198,1.83573964553602,321.849107299244));
#9904=CARTESIAN_POINT('Ctrl Pts',(-35.9255719424798,1.83573964553602,322.026461132262));
#9905=CARTESIAN_POINT('Ctrl Pts',(-35.9678797220083,1.83573964553602,322.208943590835));
#9906=CARTESIAN_POINT('Ctrl Pts',(-36.0118309030396,1.83573964553602,322.398514389896));
#9907=CARTESIAN_POINT('Ctrl Pts',(-36.0388994930129,1.83573964553602,322.593619826998));
#9908=CARTESIAN_POINT('Ctrl Pts',(-36.0492380796555,1.83573964553602,322.794372875513));
#9909=CARTESIAN_POINT('Ctrl Pts',(-36.0601918922669,1.83573964553602,323.007072285077));
#9910=CARTESIAN_POINT('Ctrl Pts',(-36.0523658257608,1.83573964553602,323.22611083602));
#9911=CARTESIAN_POINT('Ctrl Pts',(-36.0259258665584,1.83573964553602,323.451564467522));
#9912=CARTESIAN_POINT('Ctrl Pts',(-35.9978345161503,1.83573964553602,323.691099518042));
#9913=CARTESIAN_POINT('Ctrl Pts',(-35.9487323336772,1.83573964553602,323.937875220018));
#9914=CARTESIAN_POINT('Ctrl Pts',(-35.8787910094436,1.83573964553602,324.191930695693));
#9915=CARTESIAN_POINT('Ctrl Pts',(-35.8085289173363,1.83573964553602,324.447151331388));
#9916=CARTESIAN_POINT('Ctrl Pts',(-35.7172368742329,1.83573964553602,324.709717470243));
#9917=CARTESIAN_POINT('Ctrl Pts',(-35.6050496765245,1.83573964553602,324.979633431004));
#9918=CARTESIAN_POINT('Ctrl Pts',(-35.4952270641624,1.83573964553602,325.243860335095));
#9919=CARTESIAN_POINT('Ctrl Pts',(-35.3653812147248,1.83573964553602,325.515129206621));
#9920=CARTESIAN_POINT('Ctrl Pts',(-35.2155923657828,1.83573964553602,325.793428673214));
#9921=CARTESIAN_POINT('Ctrl Pts',(-35.0812280121379,1.83573964553602,326.043070273457));
#9922=CARTESIAN_POINT('Ctrl Pts',(-34.930816038242,1.83573964553602,326.298368234338));
#9923=CARTESIAN_POINT('Ctrl Pts',(-34.764378631884,1.83573964553602,326.559316446249));
#9924=CARTESIAN_POINT('',(-16.0223147731638,1.83573964553602,317.612324242706));
#9925=CARTESIAN_POINT('',(-16.022313954939,1.83573964553602,309.));
#9926=CARTESIAN_POINT('',(-33.0349479481876,1.83573964553602,325.551079813359));
#9927=CARTESIAN_POINT('Ctrl Pts',(-33.0349479481876,1.83573964553602,325.551079813359));
#9928=CARTESIAN_POINT('Ctrl Pts',(-33.0661229600418,1.83573964553602,325.502919119248));
#9929=CARTESIAN_POINT('Ctrl Pts',(-33.0982940340322,1.83573964553602,325.452411922573));
#9930=CARTESIAN_POINT('Ctrl Pts',(-33.131233956743,1.83573964553602,325.399647814597));
#9931=CARTESIAN_POINT('Ctrl Pts',(-33.1635771509031,1.83573964553602,325.347839563438));
#9932=CARTESIAN_POINT('Ctrl Pts',(-33.1966614942152,1.83573964553602,325.293855191547));
#9933=CARTESIAN_POINT('Ctrl Pts',(-33.2302370146661,1.83573964553602,325.237815505789));
#9934=CARTESIAN_POINT('Ctrl Pts',(-33.2631969912884,1.83573964553601,325.182803201953));
#9935=CARTESIAN_POINT('Ctrl Pts',(-33.2966301760354,1.83573964553601,325.125810009937));
#9936=CARTESIAN_POINT('Ctrl Pts',(-33.3302677882625,1.83573964553601,325.066988767008));
#9937=CARTESIAN_POINT('Ctrl Pts',(-33.3645508807256,1.83573964553601,325.007038789092));
#9938=CARTESIAN_POINT('Ctrl Pts',(-33.3990463607999,1.835739645536,324.945189352181));
#9939=CARTESIAN_POINT('Ctrl Pts',(-33.4334361488523,1.835739645536,324.881649213761));
#9940=CARTESIAN_POINT('Ctrl Pts',(-33.4655449686488,1.83573964553599,324.822323496158));
#9941=CARTESIAN_POINT('Ctrl Pts',(-33.4975612585259,1.83573964553599,324.761524029569));
#9942=CARTESIAN_POINT('Ctrl Pts',(-33.5292005359126,1.83573964553599,324.699463434241));
#9943=CARTESIAN_POINT('Ctrl Pts',(-33.5602287107319,1.83573964553599,324.638601519549));
#9944=CARTESIAN_POINT('Ctrl Pts',(-33.5908941148617,1.83573964553599,324.576526494744));
#9945=CARTESIAN_POINT('Ctrl Pts',(-33.6209067634036,1.83573964553598,324.513482761705));
#9946=CARTESIAN_POINT('Ctrl Pts',(-33.6503193146855,1.83573964553598,324.451699576245));
#9947=CARTESIAN_POINT('Ctrl Pts',(-33.6791047579574,1.83573964553598,324.38898581439));
#9948=CARTESIAN_POINT('Ctrl Pts',(-33.7069719015286,1.83573964553598,324.325617311444));
#9949=CARTESIAN_POINT('Ctrl Pts',(-33.7342650960075,1.83573964553598,324.26355394028));
#9950=CARTESIAN_POINT('Ctrl Pts',(-33.7606772237622,1.83573964553597,324.200862311328));
#9951=CARTESIAN_POINT('Ctrl Pts',(-33.7859199496834,1.83573964553597,324.137849069499));
#9952=CARTESIAN_POINT('Ctrl Pts',(-33.810150966544,1.83573964553597,324.077361349989));
#9953=CARTESIAN_POINT('Ctrl Pts',(-33.8333042102568,1.83573964553597,324.016577250446));
#9954=CARTESIAN_POINT('Ctrl Pts',(-33.855114095281,1.83573964553597,323.95581369679));
#9955=CARTESIAN_POINT('Ctrl Pts',(-33.8714715090491,1.83573964553597,323.910241031548));
#9956=CARTESIAN_POINT('Ctrl Pts',(-33.8870730522591,1.83573964553596,323.864680805165));
#9957=CARTESIAN_POINT('Ctrl Pts',(-33.9018036987318,1.83573964553596,323.81928501815));
#9958=CARTESIAN_POINT('Ctrl Pts',(-33.903388516175,1.83573964553596,323.814401048173));
#9959=CARTESIAN_POINT('Ctrl Pts',(-33.9049632511178,1.83573964553596,323.809518997366));
#9960=CARTESIAN_POINT('Ctrl Pts',(-33.9065277589274,1.83573964553596,323.804639066578));
#9961=CARTESIAN_POINT('Ctrl Pts',(-33.9081860973494,1.83573964553596,323.79946646426));
#9962=CARTESIAN_POINT('Ctrl Pts',(-33.9098356620974,1.83573964553597,323.794287785025));
#9963=CARTESIAN_POINT('Ctrl Pts',(-33.9114772546065,1.83573964553597,323.78909981003));
#9964=CARTESIAN_POINT('Ctrl Pts',(-33.9220168706031,1.83573964553597,323.755791139372));
#9965=CARTESIAN_POINT('Ctrl Pts',(-33.9322172469864,1.83573964553596,323.722136686936));
#9966=CARTESIAN_POINT('Ctrl Pts',(-33.9420163332251,1.83573964553596,323.688108868225));
#9967=CARTESIAN_POINT('Ctrl Pts',(-33.9515815869685,1.83573964553596,323.654893044588));
#9968=CARTESIAN_POINT('Ctrl Pts',(-33.9607644832687,1.83573964553596,323.621321202823));
#9969=CARTESIAN_POINT('Ctrl Pts',(-33.9694792291379,1.83573964553596,323.587406806218));
#9970=CARTESIAN_POINT('Ctrl Pts',(-33.9778537831925,1.83573964553596,323.554816303654));
#9971=CARTESIAN_POINT('Ctrl Pts',(-33.9857959509883,1.83573964553596,323.521909316756));
#9972=CARTESIAN_POINT('Ctrl Pts',(-33.9932039201841,1.83573964553596,323.488737145608));
#9973=CARTESIAN_POINT('Ctrl Pts',(-34.0001578485148,1.83573964553596,323.457598125635));
#9974=CARTESIAN_POINT('Ctrl Pts',(-34.0066408917444,1.83573964553596,323.426225452903));
#9975=CARTESIAN_POINT('Ctrl Pts',(-34.0125475629435,1.83573964553596,323.394697592393));
#9976=CARTESIAN_POINT('Ctrl Pts',(-34.0204218787242,1.83573964553596,323.352667094813));
#9977=CARTESIAN_POINT('Ctrl Pts',(-34.0276034892945,1.83573964553596,323.310601967879));
#9978=CARTESIAN_POINT('Ctrl Pts',(-34.0338763811083,1.83573964553596,323.268600643377));
#9979=CARTESIAN_POINT('Ctrl Pts',(-34.0402272820105,1.83573964553596,323.226076994381));
#9980=CARTESIAN_POINT('Ctrl Pts',(-34.0456467538288,1.83573964553595,323.183620856352));
#9981=CARTESIAN_POINT('Ctrl Pts',(-34.0498606505411,1.83573964553595,323.141342035231));
#9982=CARTESIAN_POINT('Ctrl Pts',(-34.0535478101644,1.83573964553595,323.10434806675));
#9983=CARTESIAN_POINT('Ctrl Pts',(-34.0563110736814,1.83573964553595,323.067491370795));
#9984=CARTESIAN_POINT('Ctrl Pts',(-34.0579366305321,1.83573964553595,323.030826699035));
#9985=CARTESIAN_POINT('Ctrl Pts',(-34.0586478116543,1.83573964553595,323.01478590514));
#9986=CARTESIAN_POINT('Ctrl Pts',(-34.0591408787633,1.83573964553595,322.998781480843));
#9987=CARTESIAN_POINT('Ctrl Pts',(-34.0593963692177,1.83573964553595,322.982815529254));
#9988=CARTESIAN_POINT('Ctrl Pts',(-34.0595457502028,1.83573964553595,322.973480505046));
#9989=CARTESIAN_POINT('Ctrl Pts',(-34.059613897403,1.83573964553595,322.964158598581));
#9990=CARTESIAN_POINT('Ctrl Pts',(-34.0595967827887,1.83573964553595,322.954849884516));
#9991=CARTESIAN_POINT('Ctrl Pts',(-34.0595895490535,1.83573964553595,322.950915424108));
#9992=CARTESIAN_POINT('Ctrl Pts',(-34.0595670825154,1.83573964553595,322.946983316998));
#9993=CARTESIAN_POINT('Ctrl Pts',(-34.0595290738543,1.83573964553595,322.943053552826));
#9994=CARTESIAN_POINT('Ctrl Pts',(-34.0594966483836,1.83573964553595,322.939701041856));
#9995=CARTESIAN_POINT('Ctrl Pts',(-34.0594528840535,1.83573964553596,322.936350674456));
#9996=CARTESIAN_POINT('Ctrl Pts',(-34.0593979182879,1.83573964553596,322.933016227715));
#9997=CARTESIAN_POINT('Ctrl Pts',(-34.0588959733313,1.83573964553596,322.902566206589));
#9998=CARTESIAN_POINT('Ctrl Pts',(-34.0574546420989,1.83573964553595,322.873152102209));
#9999=CARTESIAN_POINT('Ctrl Pts',(-34.0551137779108,1.83573964553596,322.844741632322));
#10000=CARTESIAN_POINT('Ctrl Pts',(-34.0525864883566,1.83573964553596,322.814068565452));
#10001=CARTESIAN_POINT('Ctrl Pts',(-34.0490105210139,1.83573964553596,322.784564394402));
#10002=CARTESIAN_POINT('Ctrl Pts',(-34.0444803381258,1.83573964553597,322.756139919022));
#10003=CARTESIAN_POINT('Ctrl Pts',(-34.0395034099273,1.83573964553598,322.724912355691));
#10004=CARTESIAN_POINT('Ctrl Pts',(-34.033374665099,1.83573964553598,322.694985969688));
#10005=CARTESIAN_POINT('Ctrl Pts',(-34.0262736095825,1.83573964553599,322.66620941123));
#10006=CARTESIAN_POINT('Ctrl Pts',(-34.0190897812723,1.835739645536,322.637097421492));
#10007=CARTESIAN_POINT('Ctrl Pts',(-34.0109116401738,1.83573964553601,322.609159473663));
#10008=CARTESIAN_POINT('Ctrl Pts',(-34.0019715940061,1.83573964553601,322.582244612095));
#10009=CARTESIAN_POINT('Ctrl Pts',(-33.9936074678832,1.83573964553602,322.557063612745));
#10010=CARTESIAN_POINT('Ctrl Pts',(-33.9845774637373,1.83573964553602,322.532776674166));
#10011=CARTESIAN_POINT('Ctrl Pts',(-33.9750984607969,1.83573964553602,322.509294674303));
#10012=CARTESIAN_POINT('Ctrl Pts',(-33.9715914785727,1.83573964553602,322.500606950854));
#10013=CARTESIAN_POINT('Ctrl Pts',(-33.9680232387229,1.83573964553602,322.492029864451));
#10014=CARTESIAN_POINT('Ctrl Pts',(-33.9644053373266,1.83573964553602,322.483560715069));
#10015=CARTESIAN_POINT('Ctrl Pts',(-33.9616919112793,1.83573964553602,322.477208853033));
#10016=CARTESIAN_POINT('Ctrl Pts',(-33.9589505570832,1.83573964553602,322.470917726621));
#10017=CARTESIAN_POINT('Ctrl Pts',(-33.9561862549531,1.83573964553602,322.464686624446));
#10018=CARTESIAN_POINT('Ctrl Pts',(-33.9554525044853,1.83573964553602,322.46303265396));
#10019=CARTESIAN_POINT('Ctrl Pts',(-33.9547180544517,1.83573964553602,322.461384960683));
#10020=CARTESIAN_POINT('Ctrl Pts',(-33.9539800208225,1.83573964553602,322.459736890762));
#10021=CARTESIAN_POINT('Ctrl Pts',(-33.9463767394291,1.83573964553602,322.442758342803));
#10022=CARTESIAN_POINT('Ctrl Pts',(-33.9381513961156,1.83573964553602,322.425207535287));
#10023=CARTESIAN_POINT('Ctrl Pts',(-33.9292861005445,1.83573964553602,322.407067430352));
#10024=CARTESIAN_POINT('Ctrl Pts',(-33.9163337908113,1.83573964553602,322.380564506018));
#10025=CARTESIAN_POINT('Ctrl Pts',(-33.901311364989,1.83573964553602,322.352146899478));
#10026=CARTESIAN_POINT('Ctrl Pts',(-33.8837148715601,1.83573964553602,322.321871781303));
#10027=CARTESIAN_POINT('Ctrl Pts',(-33.8661649416896,1.83573964553602,322.291676776661));
#10028=CARTESIAN_POINT('Ctrl Pts',(-33.8460516650248,1.83573964553602,322.259633661156));
#10029=CARTESIAN_POINT('Ctrl Pts',(-33.8228757301491,1.83573964553602,322.225850752003));
#10030=CARTESIAN_POINT('Ctrl Pts',(-33.8025967871328,1.83573964553602,322.196290706493));
#10031=CARTESIAN_POINT('Ctrl Pts',(-33.779971552621,1.83573964553602,322.165399323574));
#10032=CARTESIAN_POINT('Ctrl Pts',(-33.754694371687,1.83573964553602,322.133284613885));
#10033=CARTESIAN_POINT('Ctrl Pts',(-33.7324716601145,1.83573964553602,322.105050613722));
#10034=CARTESIAN_POINT('Ctrl Pts',(-33.7081987854865,1.83573964553602,322.075871552253));
#10035=CARTESIAN_POINT('Ctrl Pts',(-33.681702675014,1.83573964553602,322.045842732977));
#10036=CARTESIAN_POINT('Ctrl Pts',(-33.6586439822492,1.83573964553602,322.019709640027));
#10037=CARTESIAN_POINT('Ctrl Pts',(-33.6339015919019,1.83573964553602,321.992933294462));
#10038=CARTESIAN_POINT('Ctrl Pts',(-33.6073906529172,1.83573964553602,321.965589170075));
#10039=CARTESIAN_POINT('Ctrl Pts',(-33.5957921171115,1.83573964553602,321.953626115656));
#10040=CARTESIAN_POINT('Ctrl Pts',(-33.5838554703109,1.83573964553602,321.941554535908));
#10041=CARTESIAN_POINT('Ctrl Pts',(-33.5715756391018,1.83573964553602,321.929381449567));
#10042=CARTESIAN_POINT('Ctrl Pts',(-33.5675028306389,1.83573964553602,321.925344044799));
#10043=CARTESIAN_POINT('Ctrl Pts',(-33.5633922819587,1.83573964553602,321.921295477467));
#10044=CARTESIAN_POINT('Ctrl Pts',(-33.5592438414042,1.83573964553602,321.917236013815));
#10045=CARTESIAN_POINT('Ctrl Pts',(-33.5566208888724,1.83573964553602,321.914669319097));
#10046=CARTESIAN_POINT('Ctrl Pts',(-33.5539896374706,1.83573964553602,321.912104970658));
#10047=CARTESIAN_POINT('Ctrl Pts',(-33.5513503112792,1.83573964553602,321.90954312463));
#10048=CARTESIAN_POINT('Ctrl Pts',(-33.5083180543833,1.83573964553602,321.867774124349));
#10049=CARTESIAN_POINT('Ctrl Pts',(-33.463127010343,1.83573964553602,321.826664476558));
#10050=CARTESIAN_POINT('Ctrl Pts',(-33.4162725739017,1.83573964553602,321.786383286682));
#10051=CARTESIAN_POINT('Ctrl Pts',(-33.3665511889838,1.83573964553602,321.743637354837));
#10052=CARTESIAN_POINT('Ctrl Pts',(-33.3149589484907,1.83573964553602,321.701824351088));
#10053=CARTESIAN_POINT('Ctrl Pts',(-33.2620971297531,1.83573964553602,321.661092478806));
#10054=CARTESIAN_POINT('Ctrl Pts',(-33.2081082235734,1.83573964553602,321.619492146397));
#10055=CARTESIAN_POINT('Ctrl Pts',(-33.1527972067788,1.83573964553602,321.579019172729));
#10056=CARTESIAN_POINT('Ctrl Pts',(-33.0967785132887,1.83573964553602,321.539780381638));
#10057=CARTESIAN_POINT('Ctrl Pts',(-33.045742165131,1.83573964553602,321.50403151856));
#10058=CARTESIAN_POINT('Ctrl Pts',(-32.9941189005934,1.83573964553602,321.469306192837));
#10059=CARTESIAN_POINT('Ctrl Pts',(-32.9423350670271,1.83573964553602,321.435653391126));
#10060=CARTESIAN_POINT('Ctrl Pts',(-32.9372797495765,1.83573964553602,321.432368087895));
#10061=CARTESIAN_POINT('Ctrl Pts',(-32.9322228666748,1.83573964553602,321.429092984523));
#10062=CARTESIAN_POINT('Ctrl Pts',(-32.9271647914283,1.83573964553602,321.425828112808));
#10063=CARTESIAN_POINT('Ctrl Pts',(-32.8846896414527,1.83573964553602,321.398411376407));
#10064=CARTESIAN_POINT('Ctrl Pts',(-32.842219263063,1.83573964553602,321.371890527538));
#10065=CARTESIAN_POINT('Ctrl Pts',(-32.8000105131935,1.83573964553602,321.346250280345));
#10066=CARTESIAN_POINT('Ctrl Pts',(-32.7565769533191,1.83573964553602,321.319866006585));
#10067=CARTESIAN_POINT('Ctrl Pts',(-32.7134202611095,1.83573964553602,321.2944140929));
#10068=CARTESIAN_POINT('Ctrl Pts',(-32.670764292969,1.83573964553602,321.269868505081));
#10069=CARTESIAN_POINT('Ctrl Pts',(-32.6268132809282,1.83573964553602,321.244577708205));
#10070=CARTESIAN_POINT('Ctrl Pts',(-32.5833936843695,1.83573964553602,321.220249017716));
#10071=CARTESIAN_POINT('Ctrl Pts',(-32.5406943694291,1.83573964553602,321.196845515525));
#10072=CARTESIAN_POINT('Ctrl Pts',(-32.4966341481514,1.83573964553602,321.172696100325));
#10073=CARTESIAN_POINT('Ctrl Pts',(-32.4533406689138,1.83573964553602,321.149531703507));
#10074=CARTESIAN_POINT('Ctrl Pts',(-32.4109654673342,1.83573964553602,321.127304250182));
#10075=CARTESIAN_POINT('Ctrl Pts',(-32.3671672942411,1.83573964553602,321.10433039255));
#10076=CARTESIAN_POINT('Ctrl Pts',(-32.324349910069,1.83573964553602,321.082357379127));
#10077=CARTESIAN_POINT('Ctrl Pts',(-32.2826247223161,1.83573964553602,321.061325523161));
#10078=CARTESIAN_POINT('Ctrl Pts',(-32.2560473384883,1.83573964553602,321.047929017629));
#10079=CARTESIAN_POINT('Ctrl Pts',(-32.2299119673399,1.83573964553602,321.034914232251));
#10080=CARTESIAN_POINT('Ctrl Pts',(-32.204236776274,1.83573964553602,321.022264635838));
#10081=CARTESIAN_POINT('Ctrl Pts',(-32.1918003556014,1.83573964553602,321.016137487575));
#10082=CARTESIAN_POINT('Ctrl Pts',(-32.1794717848192,1.83573964553602,321.010096008134));
#10083=CARTESIAN_POINT('Ctrl Pts',(-32.1672524930891,1.83573964553602,321.00413825892));
#10084=CARTESIAN_POINT('Ctrl Pts',(-32.1607841646539,1.83573964553602,321.000984501771));
#10085=CARTESIAN_POINT('Ctrl Pts',(-32.1543464511367,1.83573964553602,320.997854206509));
#10086=CARTESIAN_POINT('Ctrl Pts',(-32.147939519909,1.83573964553602,320.994747081604));
#10087=CARTESIAN_POINT('Ctrl Pts',(-32.1449378300415,1.83573964553602,320.993291372932));
#10088=CARTESIAN_POINT('Ctrl Pts',(-32.1419442747369,1.83573964553602,320.991841416804));
#10089=CARTESIAN_POINT('Ctrl Pts',(-32.1389545705401,1.83573964553602,320.990395103825));
#10090=CARTESIAN_POINT('Ctrl Pts',(-32.0264733109678,1.83573964553602,320.935980655161));
#10091=CARTESIAN_POINT('Ctrl Pts',(-31.908137444516,1.83573964553602,320.881253703151));
#10092=CARTESIAN_POINT('Ctrl Pts',(-31.7837893774404,1.83573964553602,320.826251984166));
#10093=CARTESIAN_POINT('Ctrl Pts',(-31.6585403111675,1.83573964553602,320.770851734623));
#10094=CARTESIAN_POINT('Ctrl Pts',(-31.5271915179057,1.83573964553602,320.715172504509));
#10095=CARTESIAN_POINT('Ctrl Pts',(-31.3895291454136,1.83573964553602,320.659258824958));
#10096=CARTESIAN_POINT('Ctrl Pts',(-31.2510604150361,1.83573964553602,320.60301763081));
#10097=CARTESIAN_POINT('Ctrl Pts',(-31.1062038344124,1.83573964553602,320.546538993237));
#10098=CARTESIAN_POINT('Ctrl Pts',(-30.9546898749326,1.83573964553602,320.489877692076));
#10099=CARTESIAN_POINT('Ctrl Pts',(-30.8022990163583,1.83573964553602,320.432888459126));
#10100=CARTESIAN_POINT('Ctrl Pts',(-30.6431734062554,1.83573964553602,320.375714174219));
#10101=CARTESIAN_POINT('Ctrl Pts',(-30.4769878213684,1.83573964553602,320.318423942592));
#10102=CARTESIAN_POINT('Ctrl Pts',(-30.3105628359861,1.83573964553602,320.261051180884));
#10103=CARTESIAN_POINT('Ctrl Pts',(-30.1370573939087,1.83573964553602,320.203561852257));
#10104=CARTESIAN_POINT('Ctrl Pts',(-29.9560955534919,1.83573964553602,320.146042878496));
#10105=CARTESIAN_POINT('Ctrl Pts',(-29.7752986487112,1.83573964553602,320.088576329758));
#10106=CARTESIAN_POINT('Ctrl Pts',(-29.5870587823504,1.83573964553602,320.031079883726));
#10107=CARTESIAN_POINT('Ctrl Pts',(-29.3909539457544,1.83573964553602,319.973662122803));
#10108=CARTESIAN_POINT('Ctrl Pts',(-29.2776290644937,1.83573964553602,319.940481600325));
#10109=CARTESIAN_POINT('Ctrl Pts',(-29.1616768600902,1.83573964553602,319.907327782954));
#10110=CARTESIAN_POINT('Ctrl Pts',(-29.043009016516,1.83573964553602,319.874225600227));
#10111=CARTESIAN_POINT('Ctrl Pts',(-28.8007656894285,1.83573964553602,319.80665225739));
#10112=CARTESIAN_POINT('Ctrl Pts',(-28.5473824685975,1.83573964553602,319.739066503176));
#10113=CARTESIAN_POINT('Ctrl Pts',(-28.2822169710412,1.83573964553602,319.671421318884));
#10114=CARTESIAN_POINT('Ctrl Pts',(-27.9983427087817,1.83573964553602,319.599003425291));
#10115=CARTESIAN_POINT('Ctrl Pts',(-27.700964380257,1.83573964553602,319.526517177977));
#10116=CARTESIAN_POINT('Ctrl Pts',(-27.3892358081502,1.83573964553602,319.453922151971));
#10117=CARTESIAN_POINT('Ctrl Pts',(-27.0354358203731,1.83573964553602,319.371529578393));
#10118=CARTESIAN_POINT('Ctrl Pts',(-26.663149516191,1.83573964553602,319.288996201745));
#10119=CARTESIAN_POINT('Ctrl Pts',(-26.271080031633,1.83573964553602,319.206292236006));
#10120=CARTESIAN_POINT('Ctrl Pts',(-25.8610062347746,1.83573964553602,319.119790402576));
#10121=CARTESIAN_POINT('Ctrl Pts',(-25.429286642215,1.83573964553602,319.033101515975));
#10122=CARTESIAN_POINT('Ctrl Pts',(-24.9744178788053,1.83573964553602,318.946230143728));
#10123=CARTESIAN_POINT('Ctrl Pts',(-24.6003130682804,1.83573964553602,318.874783166338));
#10124=CARTESIAN_POINT('Ctrl Pts',(-24.2105479126315,1.83573964553602,318.803213426619));
#10125=CARTESIAN_POINT('Ctrl Pts',(-23.8043103135764,1.83573964553602,318.731544709485));
#10126=CARTESIAN_POINT('Ctrl Pts',(-23.4432514353454,1.83573964553602,318.667846453407));
#10127=CARTESIAN_POINT('Ctrl Pts',(-23.0691794360944,1.83573964553602,318.604070244179));
#10128=CARTESIAN_POINT('Ctrl Pts',(-22.6815611843081,1.83573964553602,318.540246192317));
#10129=CARTESIAN_POINT('Ctrl Pts',(-22.3248548638107,1.83573964553602,318.481512005797));
#10130=CARTESIAN_POINT('Ctrl Pts',(-21.9566761681602,1.83573964553602,318.422737416197));
#10131=CARTESIAN_POINT('Ctrl Pts',(-21.5766520973531,1.83573964553602,318.363955779299));
#10132=CARTESIAN_POINT('Ctrl Pts',(-21.2206131023023,1.83573964553602,318.308884123221));
#10133=CARTESIAN_POINT('Ctrl Pts',(-20.8541763488,1.83573964553602,318.253806348451));
#10134=CARTESIAN_POINT('Ctrl Pts',(-20.477080807384,1.83573964553602,318.198757752451));
#10135=CARTESIAN_POINT('Ctrl Pts',(-20.1284259143964,1.83573964553602,318.147860936553));
#10136=CARTESIAN_POINT('Ctrl Pts',(-19.7706592399563,1.83573964553602,318.096989131011));
#10137=CARTESIAN_POINT('Ctrl Pts',(-19.4036184737005,1.83573964553602,318.046176242108));
#10138=CARTESIAN_POINT('Ctrl Pts',(-19.0501707445755,1.83573964553602,317.99724516457));
#10139=CARTESIAN_POINT('Ctrl Pts',(-18.6881227696217,1.83573964553602,317.948368742741));
#10140=CARTESIAN_POINT('Ctrl Pts',(-18.3173759377902,1.83573964553602,317.899582486812));
#10141=CARTESIAN_POINT('Ctrl Pts',(-17.9656988419601,1.83573964553602,317.853305601002));
#10142=CARTESIAN_POINT('Ctrl Pts',(-17.6061945905643,1.83573964553602,317.807109874995));
#10143=CARTESIAN_POINT('Ctrl Pts',(-17.238824839512,1.83573964553602,317.761030019511));
#10144=CARTESIAN_POINT('Ctrl Pts',(-16.9638795440795,1.83573964553602,317.726543131456));
#10145=CARTESIAN_POINT('Ctrl Pts',(-16.684529436466,1.83573964553602,317.692121232857));
#10146=CARTESIAN_POINT('Ctrl Pts',(-16.4007776292659,1.83573964553602,317.65778048784));
#10147=CARTESIAN_POINT('Ctrl Pts',(-16.2754547949549,1.83573964553602,317.642613432023));
#10148=CARTESIAN_POINT('Ctrl Pts',(-16.1493020013402,1.83573964553602,317.627460892713));
#10149=CARTESIAN_POINT('Ctrl Pts',(-16.0223151822762,1.83573964553602,317.612324258224));
#10150=CARTESIAN_POINT('',(-23.9503331469548,1.83573964553602,320.25486209));
#10151=CARTESIAN_POINT('Origin',(-16.022313954939,-1.83573964553602,309.));
#10152=CARTESIAN_POINT('',(-16.022313954939,-1.83573964553602,315.598323807971));
#10153=CARTESIAN_POINT('',(-16.022313954939,-1.83573964553602,315.598323807971));
#10154=CARTESIAN_POINT('',(-16.0223147731638,-1.83573964553602,317.612324242706));
#10155=CARTESIAN_POINT('',(-16.022313954939,-1.83573964553602,309.));
#10156=CARTESIAN_POINT('',(-16.0223151822762,1.83573964553602,317.612324258224));
#10157=CARTESIAN_POINT('Origin',(-40.3518529101985,-1.83573964553602,309.));
#10158=CARTESIAN_POINT('',(-34.7643786318829,-1.83573964553602,326.55931644625));
#10159=CARTESIAN_POINT('Ctrl Pts',(-34.764378631884,-1.83573964553602,326.559316446249));
#10160=CARTESIAN_POINT('Ctrl Pts',(-34.919829498708,-1.83573964553602,326.315593435747));
#10161=CARTESIAN_POINT('Ctrl Pts',(-35.0709574919393,-1.83573964553603,
326.06166299344));
#10162=CARTESIAN_POINT('Ctrl Pts',(-35.2117363266656,-1.83573964553605,
325.800586363758));
#10163=CARTESIAN_POINT('Ctrl Pts',(-35.3429176445163,-1.83573964553607,
325.557308484605));
#10164=CARTESIAN_POINT('Ctrl Pts',(-35.4651065858305,-1.83573964553609,
325.307828880366));
#10165=CARTESIAN_POINT('Ctrl Pts',(-35.5734293953103,-1.8357396455361,325.054611439063));
#10166=CARTESIAN_POINT('Ctrl Pts',(-35.624205712254,-1.83573964553611,324.935915763452));
#10167=CARTESIAN_POINT('Ctrl Pts',(-35.6719358463144,-1.83573964553612,
324.816398306841));
#10168=CARTESIAN_POINT('Ctrl Pts',(-35.7161231976916,-1.83573964553612,
324.696308546926));
#10169=CARTESIAN_POINT('Ctrl Pts',(-35.7375264460149,-1.83573964553612,
324.638140069467));
#10170=CARTESIAN_POINT('Ctrl Pts',(-35.7580985605365,-1.83573964553612,
324.579837262752));
#10171=CARTESIAN_POINT('Ctrl Pts',(-35.7777835675407,-1.83573964553612,
324.521428110438));
#10172=CARTESIAN_POINT('Ctrl Pts',(-35.790121733712,-1.83573964553613,324.484818429424));
#10173=CARTESIAN_POINT('Ctrl Pts',(-35.8021114034735,-1.83573964553613,
324.448166965075));
#10174=CARTESIAN_POINT('Ctrl Pts',(-35.8137388658144,-1.83573964553613,
324.411480550089));
#10175=CARTESIAN_POINT('Ctrl Pts',(-35.8199545189524,-1.83573964553613,
324.391869217561));
#10176=CARTESIAN_POINT('Ctrl Pts',(-35.8260666681465,-1.83573964553613,
324.372247896694));
#10177=CARTESIAN_POINT('Ctrl Pts',(-35.832073225929,-1.83573964553613,324.352617625523));
#10178=CARTESIAN_POINT('Ctrl Pts',(-35.8354794513467,-1.83573964553613,
324.341485604316));
#10179=CARTESIAN_POINT('Ctrl Pts',(-35.8388527537894,-1.83573964553612,
324.330347382553));
#10180=CARTESIAN_POINT('Ctrl Pts',(-35.842195044056,-1.83573964553612,324.319195126364));
#10181=CARTESIAN_POINT('Ctrl Pts',(-35.904156576116,-1.83573964553612,324.112447410186));
#10182=CARTESIAN_POINT('Ctrl Pts',(-35.955206972034,-1.83573964553613,323.901705493671));
#10183=CARTESIAN_POINT('Ctrl Pts',(-35.991654591359,-1.83573964553613,323.688750751308));
#10184=CARTESIAN_POINT('Ctrl Pts',(-36.0214654326083,-1.83573964553613,
323.514573119533));
#10185=CARTESIAN_POINT('Ctrl Pts',(-36.0415060533855,-1.83573964553613,
323.33891554914));
#10186=CARTESIAN_POINT('Ctrl Pts',(-36.0497684509554,-1.83573964553613,
323.162717079327));
#10187=CARTESIAN_POINT('Ctrl Pts',(-36.0522529480809,-1.83573964553613,
323.109734323647));
#10188=CARTESIAN_POINT('Ctrl Pts',(-36.0536726122713,-1.83573964553613,
323.056702357695));
#10189=CARTESIAN_POINT('Ctrl Pts',(-36.0539733280531,-1.83573964553613,
323.003645833575));
#10190=CARTESIAN_POINT('Ctrl Pts',(-36.0541436617393,-1.83573964553613,
322.973593159648));
#10191=CARTESIAN_POINT('Ctrl Pts',(-36.0539549967846,-1.83573964553613,
322.943532598032));
#10192=CARTESIAN_POINT('Ctrl Pts',(-36.0533975407004,-1.83573964553613,
322.913468557433));
#10193=CARTESIAN_POINT('Ctrl Pts',(-36.0530871771216,-1.83573964553613,
322.896730408008));
#10194=CARTESIAN_POINT('Ctrl Pts',(-36.0526624997886,-1.83573964553613,
322.879991179246));
#10195=CARTESIAN_POINT('Ctrl Pts',(-36.0521218232439,-1.83573964553613,
322.863251624484));
#10196=CARTESIAN_POINT('Ctrl Pts',(-36.0517128308649,-1.83573964553613,
322.850589062382));
#10197=CARTESIAN_POINT('Ctrl Pts',(-36.0512373152779,-1.83573964553613,
322.83792418292));
#10198=CARTESIAN_POINT('Ctrl Pts',(-36.0506956710076,-1.83573964553613,
322.825279591146));
#10199=CARTESIAN_POINT('Ctrl Pts',(-36.0428318976773,-1.83573964553613,
322.641701163372));
#10200=CARTESIAN_POINT('Ctrl Pts',(-36.0210023687523,-1.83573964553613,
322.461375790017));
#10201=CARTESIAN_POINT('Ctrl Pts',(-35.984438433772,-1.83573964553612,322.284478185075));
#10202=CARTESIAN_POINT('Ctrl Pts',(-35.9498008213356,-1.83573964553611,
322.116900196432));
#10203=CARTESIAN_POINT('Ctrl Pts',(-35.9019401767507,-1.83573964553611,
321.952398681821));
#10204=CARTESIAN_POINT('Ctrl Pts',(-35.8402013746489,-1.83573964553611,
321.791073726073));
#10205=CARTESIAN_POINT('Ctrl Pts',(-35.8239901926768,-1.83573964553611,
321.74871352268));
#10206=CARTESIAN_POINT('Ctrl Pts',(-35.8068221660236,-1.83573964553611,
321.706572051959));
#10207=CARTESIAN_POINT('Ctrl Pts',(-35.7886854810261,-1.83573964553611,
321.664650526461));
#10208=CARTESIAN_POINT('Ctrl Pts',(-35.7836966569188,-1.83573964553611,
321.653119250649));
#10209=CARTESIAN_POINT('Ctrl Pts',(-35.7786345419672,-1.83573964553611,
321.641604614989));
#10210=CARTESIAN_POINT('Ctrl Pts',(-35.7734988909164,-1.83573964553611,
321.630106641422));
#10211=CARTESIAN_POINT('Ctrl Pts',(-35.7700958011473,-1.83573964553611,
321.622487619837));
#10212=CARTESIAN_POINT('Ctrl Pts',(-35.7666637923649,-1.83573964553611,
321.614883486877));
#10213=CARTESIAN_POINT('Ctrl Pts',(-35.7632047952331,-1.83573964553611,
321.60729809249));
#10214=CARTESIAN_POINT('Ctrl Pts',(-35.6868709731977,-1.83573964553611,
321.439902132573));
#10215=CARTESIAN_POINT('Ctrl Pts',(-35.5971163415451,-1.83573964553611,
321.281019102654));
#10216=CARTESIAN_POINT('Ctrl Pts',(-35.4959479809854,-1.83573964553611,
321.12997587918));
#10217=CARTESIAN_POINT('Ctrl Pts',(-35.4039568383216,-1.83573964553611,
320.992634138717));
#10218=CARTESIAN_POINT('Ctrl Pts',(-35.3025298409702,-1.83573964553611,
320.861773652812));
#10219=CARTESIAN_POINT('Ctrl Pts',(-35.1932091120446,-1.83573964553611,
320.736906185937));
#10220=CARTESIAN_POINT('Ctrl Pts',(-35.1419650203607,-1.83573964553611,
320.678374560839));
#10221=CARTESIAN_POINT('Ctrl Pts',(-35.0889868731899,-1.83573964553611,
320.621160091195));
#10222=CARTESIAN_POINT('Ctrl Pts',(-35.0344353428421,-1.83573964553611,
320.565214563772));
#10223=CARTESIAN_POINT('Ctrl Pts',(-35.0080119453299,-1.83573964553611,
320.538115948927));
#10224=CARTESIAN_POINT('Ctrl Pts',(-34.9812194168613,-1.83573964553611,
320.511315074697));
#10225=CARTESIAN_POINT('Ctrl Pts',(-34.9540760904638,-1.83573964553611,
320.484806595523));
#10226=CARTESIAN_POINT('Ctrl Pts',(-34.9452697370927,-1.83573964553611,
320.476206211343));
#10227=CARTESIAN_POINT('Ctrl Pts',(-34.9364264588272,-1.83573964553611,
320.467636605576));
#10228=CARTESIAN_POINT('Ctrl Pts',(-34.9275468826458,-1.83573964553611,
320.459097597761));
#10229=CARTESIAN_POINT('Ctrl Pts',(-34.9182349861886,-1.83573964553611,
320.450142850936));
#10230=CARTESIAN_POINT('Ctrl Pts',(-34.9088882279726,-1.83573964553611,
320.441226479291));
#10231=CARTESIAN_POINT('Ctrl Pts',(-34.8994801179544,-1.83573964553611,
320.432322702167));
#10232=CARTESIAN_POINT('Ctrl Pts',(-34.7581536133364,-1.83573964553611,
320.298572172423));
#10233=CARTESIAN_POINT('Ctrl Pts',(-34.6038513564271,-1.8357396455361,320.168510760348));
#10234=CARTESIAN_POINT('Ctrl Pts',(-34.4364491814111,-1.83573964553609,
320.041799621155));
#10235=CARTESIAN_POINT('Ctrl Pts',(-34.2593578809453,-1.83573964553607,
319.907754526335));
#10236=CARTESIAN_POINT('Ctrl Pts',(-34.0676058937315,-1.83573964553606,
319.777458308624));
#10237=CARTESIAN_POINT('Ctrl Pts',(-33.8609893372873,-1.83573964553604,
319.650529883203));
#10238=CARTESIAN_POINT('Ctrl Pts',(-33.635098772893,-1.83573964553603,319.511761073242));
#10239=CARTESIAN_POINT('Ctrl Pts',(-33.391439573106,-1.83573964553602,319.377016777585));
#10240=CARTESIAN_POINT('Ctrl Pts',(-33.1296933633902,-1.83573964553601,
319.245833289073));
#10241=CARTESIAN_POINT('Ctrl Pts',(-33.066169688179,-1.83573964553601,319.21399612388));
#10242=CARTESIAN_POINT('Ctrl Pts',(-33.0015805470171,-1.83573964553601,
319.182368871595));
#10243=CARTESIAN_POINT('Ctrl Pts',(-32.9359211723264,-1.83573964553601,
319.15094527135));
#10244=CARTESIAN_POINT('Ctrl Pts',(-32.927382150455,-1.83573964553601,319.146858622474));
#10245=CARTESIAN_POINT('Ctrl Pts',(-32.9188288323849,-1.83573964553601,
319.142777214983));
#10246=CARTESIAN_POINT('Ctrl Pts',(-32.9102355177821,-1.83573964553601,
319.138688853223));
#10247=CARTESIAN_POINT('Ctrl Pts',(-32.7983897862637,-1.83573964553601,
319.085477044647));
#10248=CARTESIAN_POINT('Ctrl Pts',(-32.6805626663053,-1.83573964553601,
319.031466453008));
#10249=CARTESIAN_POINT('Ctrl Pts',(-32.5560947943014,-1.83573964553601,
318.976659291702));
#10250=CARTESIAN_POINT('Ctrl Pts',(-32.4312856481312,-1.83573964553601,
318.921701856531));
#10251=CARTESIAN_POINT('Ctrl Pts',(-32.2997992729873,-1.83573964553601,
318.865943489233));
#10252=CARTESIAN_POINT('Ctrl Pts',(-32.1609188082923,-1.83573964553601,
318.809392801681));
#10253=CARTESIAN_POINT('Ctrl Pts',(-32.0194975723913,-1.83573964553601,
318.751807538397));
#10254=CARTESIAN_POINT('Ctrl Pts',(-31.8704092594458,-1.83573964553601,
318.693400697781));
#10255=CARTESIAN_POINT('Ctrl Pts',(-31.7128425891105,-1.83573964553601,
318.634187910249));
#10256=CARTESIAN_POINT('Ctrl Pts',(-31.5511994143238,-1.83573964553601,
318.573443192193));
#10257=CARTESIAN_POINT('Ctrl Pts',(-31.3806334401196,-1.83573964553601,
318.511850269096));
#10258=CARTESIAN_POINT('Ctrl Pts',(-31.200212177051,-1.83573964553601,318.44943297343));
#10259=CARTESIAN_POINT('Ctrl Pts',(-31.0112459120662,-1.83573964553601,
318.384059507842));
#10260=CARTESIAN_POINT('Ctrl Pts',(-30.8114685442404,-1.83573964553601,
318.317781667008));
#10261=CARTESIAN_POINT('Ctrl Pts',(-30.5997488998527,-1.83573964553601,
318.250635026041));
#10262=CARTESIAN_POINT('Ctrl Pts',(-30.3701849676304,-1.83573964553601,
318.177829089775));
#10263=CARTESIAN_POINT('Ctrl Pts',(-30.126580348697,-1.83573964553601,318.104001539579));
#10264=CARTESIAN_POINT('Ctrl Pts',(-29.867429065394,-1.83573964553601,318.029209289024));
#10265=CARTESIAN_POINT('Ctrl Pts',(-29.5544940093786,-1.83573964553601,
317.938894794655));
#10266=CARTESIAN_POINT('Ctrl Pts',(-29.2188882099064,-1.83573964553601,
317.847172910493));
#10267=CARTESIAN_POINT('Ctrl Pts',(-28.8578814451977,-1.83573964553601,
317.754167971317));
#10268=CARTESIAN_POINT('Ctrl Pts',(-28.5298192834568,-1.83573964553601,
317.669650437627));
#10269=CARTESIAN_POINT('Ctrl Pts',(-28.1807761284515,-1.83573964553601,
317.584073620011));
#10270=CARTESIAN_POINT('Ctrl Pts',(-27.8086957725647,-1.83573964553601,
317.497550185639));
#10271=CARTESIAN_POINT('Ctrl Pts',(-27.4831254611637,-1.83573964553601,
317.421842180563));
#10272=CARTESIAN_POINT('Ctrl Pts',(-27.1399151008274,-1.83573964553601,
317.345409648215));
#10273=CARTESIAN_POINT('Ctrl Pts',(-26.7777227702123,-1.83573964553602,
317.268340184405));
#10274=CARTESIAN_POINT('Ctrl Pts',(-26.4608044809241,-1.83573964553602,
317.200904403571));
#10275=CARTESIAN_POINT('Ctrl Pts',(-26.1293523138813,-1.83573964553602,
317.132981084406));
#10276=CARTESIAN_POINT('Ctrl Pts',(-25.7825143870751,-1.83573964553602,
317.064636847793));
#10277=CARTESIAN_POINT('Ctrl Pts',(-25.4790312011196,-1.83573964553602,
317.004835640756));
#10278=CARTESIAN_POINT('Ctrl Pts',(-25.1637682058098,-1.83573964553602,
316.944712240703));
#10279=CARTESIAN_POINT('Ctrl Pts',(-24.8361981433063,-1.83573964553602,
316.884316639796));
#10280=CARTESIAN_POINT('Ctrl Pts',(-24.530513916328,-1.83573964553602,316.82795623117));
#10281=CARTESIAN_POINT('Ctrl Pts',(-24.214111964592,-1.83573964553601,316.771358791136));
#10282=CARTESIAN_POINT('Ctrl Pts',(-23.8866071050454,-1.83573964553602,
316.714569487522));
#10283=CARTESIAN_POINT('Ctrl Pts',(-23.5723176576479,-1.83573964553602,
316.660071734799));
#10284=CARTESIAN_POINT('Ctrl Pts',(-23.2478029725362,-1.83573964553601,
316.605397287888));
#10285=CARTESIAN_POINT('Ctrl Pts',(-22.9127680347174,-1.83573964553602,
316.550590348815));
#10286=CARTESIAN_POINT('Ctrl Pts',(-22.5888443425662,-1.83573964553602,
316.497601051114));
#10287=CARTESIAN_POINT('Ctrl Pts',(-22.2550863795048,-1.83573964553602,
316.444487898802));
#10288=CARTESIAN_POINT('Ctrl Pts',(-21.9112747750118,-1.83573964553602,
316.39129498806));
#10289=CARTESIAN_POINT('Ctrl Pts',(-21.5769144833199,-1.83573964553602,
316.339564339883));
#10290=CARTESIAN_POINT('Ctrl Pts',(-21.2330455008927,-1.83573964553602,
316.287758252604));
#10291=CARTESIAN_POINT('Ctrl Pts',(-20.879514750595,-1.83573964553602,316.235921354704));
#10292=CARTESIAN_POINT('Ctrl Pts',(-20.5342625107455,-1.83573964553602,
316.185298303975));
#10293=CARTESIAN_POINT('Ctrl Pts',(-20.1797955310403,-1.83573964553602,
316.13464586032));
#10294=CARTESIAN_POINT('Ctrl Pts',(-19.8160210095592,-1.83573964553602,
316.084009629196));
#10295=CARTESIAN_POINT('Ctrl Pts',(-19.46163404477,-1.83573964553602,316.034680115454));
#10296=CARTESIAN_POINT('Ctrl Pts',(-19.098413653549,-1.83573964553602,315.985365984819));
#10297=CARTESIAN_POINT('Ctrl Pts',(-18.7263234961891,-1.83573964553602,
315.936113366434));
#10298=CARTESIAN_POINT('Ctrl Pts',(-18.3582593515104,-1.83573964553602,
315.887393661007));
#10299=CARTESIAN_POINT('Ctrl Pts',(-17.9815162269729,-1.83573964553602,
315.83873413412));
#10300=CARTESIAN_POINT('Ctrl Pts',(-17.596109528008,-1.83573964553602,315.790183476892));
#10301=CARTESIAN_POINT('Ctrl Pts',(-17.2136841826627,-1.83573964553602,
315.742008388325));
#10302=CARTESIAN_POINT('Ctrl Pts',(-16.8227287332923,-1.83573964553602,
315.693940487264));
#10303=CARTESIAN_POINT('Ctrl Pts',(-16.423309601714,-1.83573964553602,315.646031462909));
#10304=CARTESIAN_POINT('Ctrl Pts',(-16.2905773856919,-1.83573964553602,
315.630110665763));
#10305=CARTESIAN_POINT('Ctrl Pts',(-16.15691093349,-1.83573964553602,315.614207447801));
#10306=CARTESIAN_POINT('Ctrl Pts',(-16.022313954939,-1.83573964553602,315.598323807971));
#10307=CARTESIAN_POINT('',(-33.0349479481876,-1.83573964553602,325.551079813359));
#10308=CARTESIAN_POINT('',(-33.0293694032794,-1.83573964553602,325.547827590886));
#10309=CARTESIAN_POINT('Ctrl Pts',(-16.0223151822761,-1.83573964553602,
317.612324258224));
#10310=CARTESIAN_POINT('Ctrl Pts',(-16.1477973978183,-1.83573964553602,
317.627281546276));
#10311=CARTESIAN_POINT('Ctrl Pts',(-16.2739661013669,-1.83573964553602,
317.642433264547));
#10312=CARTESIAN_POINT('Ctrl Pts',(-16.4007776292659,-1.83573964553602,
317.65778048784));
#10313=CARTESIAN_POINT('Ctrl Pts',(-16.7384550918035,-1.83573964553602,
317.698647524965));
#10314=CARTESIAN_POINT('Ctrl Pts',(-17.0804884887966,-1.83573964553603,
317.740910768462));
#10315=CARTESIAN_POINT('Ctrl Pts',(-17.4258778156812,-1.83573964553603,
317.784588179341));
#10316=CARTESIAN_POINT('Ctrl Pts',(-17.7806192669341,-1.83573964553604,
317.829448245696));
#10317=CARTESIAN_POINT('Ctrl Pts',(-18.1389006976833,-1.83573964553604,
317.87580016583));
#10318=CARTESIAN_POINT('Ctrl Pts',(-18.4995828290648,-1.83573964553605,
317.923658900772));
#10319=CARTESIAN_POINT('Ctrl Pts',(-18.8743379902158,-1.83573964553605,
317.973384979125));
#10320=CARTESIAN_POINT('Ctrl Pts',(-19.2516846085092,-1.83573964553607,
318.024737842581));
#10321=CARTESIAN_POINT('Ctrl Pts',(-19.6302880901341,-1.83573964553608,
318.077728238319));
#10322=CARTESIAN_POINT('Ctrl Pts',(-20.0308257740179,-1.83573964553609,
318.133788605978));
#10323=CARTESIAN_POINT('Ctrl Pts',(-20.4327697742083,-1.8357396455361,318.19168188436));
#10324=CARTESIAN_POINT('Ctrl Pts',(-20.834482210606,-1.83573964553611,318.251412294469));
#10325=CARTESIAN_POINT('Ctrl Pts',(-21.303558974513,-1.83573964553612,318.321159070876));
#10326=CARTESIAN_POINT('Ctrl Pts',(-21.7723197118664,-1.83573964553613,
318.39341130996));
#10327=CARTESIAN_POINT('Ctrl Pts',(-22.23808360911,-1.83573964553615,318.468158799972));
#10328=CARTESIAN_POINT('Ctrl Pts',(-22.8064091100986,-1.83573964553616,
318.559365750447));
#10329=CARTESIAN_POINT('Ctrl Pts',(-23.3702689307725,-1.83573964553617,
318.654289363245));
#10330=CARTESIAN_POINT('Ctrl Pts',(-23.9247188275741,-1.83573964553618,
318.752869991931));
#10331=CARTESIAN_POINT('Ctrl Pts',(-24.3988170855096,-1.83573964553619,
318.837164180813));
#10332=CARTESIAN_POINT('Ctrl Pts',(-24.8660306052653,-1.8357396455362,318.924131605397));
#10333=CARTESIAN_POINT('Ctrl Pts',(-25.3232865256788,-1.8357396455362,319.013706084701));
#10334=CARTESIAN_POINT('Ctrl Pts',(-25.4090220107563,-1.8357396455362,319.030501299571));
#10335=CARTESIAN_POINT('Ctrl Pts',(-25.4944075808075,-1.8357396455362,319.047388089524));
#10336=CARTESIAN_POINT('Ctrl Pts',(-25.5794232403297,-1.8357396455362,319.064365907288));
#10337=CARTESIAN_POINT('Ctrl Pts',(-25.6227005251825,-1.8357396455362,319.073008478076));
#10338=CARTESIAN_POINT('Ctrl Pts',(-25.6658819558488,-1.8357396455362,319.081674636569));
#10339=CARTESIAN_POINT('Ctrl Pts',(-25.7089649060401,-1.8357396455362,319.090364306988));
#10340=CARTESIAN_POINT('Ctrl Pts',(-25.7317114794517,-1.8357396455362,319.094952206034));
#10341=CARTESIAN_POINT('Ctrl Pts',(-25.7544306011717,-1.8357396455362,319.099546659082));
#10342=CARTESIAN_POINT('Ctrl Pts',(-25.7771218856057,-1.8357396455362,319.104147654706));
#10343=CARTESIAN_POINT('Ctrl Pts',(-25.798394351303,-1.8357396455362,319.108460963715));
#10344=CARTESIAN_POINT('Ctrl Pts',(-25.8196336740054,-1.8357396455362,319.112778264217));
#10345=CARTESIAN_POINT('Ctrl Pts',(-25.8408363513149,-1.8357396455362,319.117098867872));
#10346=CARTESIAN_POINT('Ctrl Pts',(-26.117190526685,-1.8357396455362,319.173413306037));
#10347=CARTESIAN_POINT('Ctrl Pts',(-26.3875181930021,-1.8357396455362,319.230327749865));
#10348=CARTESIAN_POINT('Ctrl Pts',(-26.6518879881453,-1.8357396455362,319.287913666536));
#10349=CARTESIAN_POINT('Ctrl Pts',(-26.9038922118028,-1.8357396455362,319.342806072897));
#10350=CARTESIAN_POINT('Ctrl Pts',(-27.1504829743502,-1.8357396455362,319.398308654903));
#10351=CARTESIAN_POINT('Ctrl Pts',(-27.3916728179156,-1.8357396455362,319.454489746202));
#10352=CARTESIAN_POINT('Ctrl Pts',(-27.6271052020578,-1.8357396455362,319.509329734788));
#10353=CARTESIAN_POINT('Ctrl Pts',(-27.8573916738498,-1.8357396455362,319.564816243724));
#10354=CARTESIAN_POINT('Ctrl Pts',(-28.0824954546864,-1.8357396455362,319.621018670888));
#10355=CARTESIAN_POINT('Ctrl Pts',(-28.3002562087911,-1.8357396455362,319.675387739575));
#10356=CARTESIAN_POINT('Ctrl Pts',(-28.5131670000565,-1.8357396455362,319.730426803238));
#10357=CARTESIAN_POINT('Ctrl Pts',(-28.7211462451106,-1.8357396455362,319.786203917586));
#10358=CARTESIAN_POINT('Ctrl Pts',(-28.8297860424903,-1.8357396455362,319.815339586386));
#10359=CARTESIAN_POINT('Ctrl Pts',(-28.9370794045402,-1.8357396455362,319.844676724422));
#10360=CARTESIAN_POINT('Ctrl Pts',(-29.043009016516,-1.8357396455362,319.874225600227));
#10361=CARTESIAN_POINT('Ctrl Pts',(-29.2397507640582,-1.8357396455362,319.92910635883));
#10362=CARTESIAN_POINT('Ctrl Pts',(-29.4316765956865,-1.8357396455362,319.98486773198));
#10363=CARTESIAN_POINT('Ctrl Pts',(-29.6187127167007,-1.8357396455362,320.041439421539));
#10364=CARTESIAN_POINT('Ctrl Pts',(-29.8024953509048,-1.8357396455362,320.097027048528));
#10365=CARTESIAN_POINT('Ctrl Pts',(-29.9815570165904,-1.8357396455362,320.153397216642));
#10366=CARTESIAN_POINT('Ctrl Pts',(-30.1557786611949,-1.8357396455362,320.210481790954));
#10367=CARTESIAN_POINT('Ctrl Pts',(-30.3269354514096,-1.8357396455362,320.266562150729));
#10368=CARTESIAN_POINT('Ctrl Pts',(-30.4934211174452,-1.8357396455362,320.323332157974));
#10369=CARTESIAN_POINT('Ctrl Pts',(-30.6550734539028,-1.8357396455362,320.380723420614));
#10370=CARTESIAN_POINT('Ctrl Pts',(-30.813866991154,-1.8357396455362,320.437099726714));
#10371=CARTESIAN_POINT('Ctrl Pts',(-30.9679967454257,-1.8357396455362,320.49407565197));
#10372=CARTESIAN_POINT('Ctrl Pts',(-31.1172593976607,-1.8357396455362,320.551580492726));
#10373=CARTESIAN_POINT('Ctrl Pts',(-31.2638800782195,-1.8357396455362,320.608067489043));
#10374=CARTESIAN_POINT('Ctrl Pts',(-31.4058045324441,-1.8357396455362,320.665064975756));
#10375=CARTESIAN_POINT('Ctrl Pts',(-31.542790261857,-1.8357396455362,320.722498194282));
#10376=CARTESIAN_POINT('Ctrl Pts',(-31.5984863479931,-1.8357396455362,320.745849571829));
#10377=CARTESIAN_POINT('Ctrl Pts',(-31.6533654258363,-1.8357396455362,320.769272878874));
#10378=CARTESIAN_POINT('Ctrl Pts',(-31.7074087147834,-1.8357396455362,320.792762636528));
#10379=CARTESIAN_POINT('Ctrl Pts',(-31.7310526536978,-1.8357396455362,320.803039405501));
#10380=CARTESIAN_POINT('Ctrl Pts',(-31.7545365983725,-1.8357396455362,320.813328889837));
#10381=CARTESIAN_POINT('Ctrl Pts',(-31.7778588863295,-1.8357396455362,320.823630612852));
#10382=CARTESIAN_POINT('Ctrl Pts',(-31.7887912088093,-1.8357396455362,320.828459545515));
#10383=CARTESIAN_POINT('Ctrl Pts',(-31.7996880102247,-1.8357396455362,320.833291167181));
#10384=CARTESIAN_POINT('Ctrl Pts',(-31.8105491151427,-1.8357396455362,320.838125427887));
#10385=CARTESIAN_POINT('Ctrl Pts',(-31.8186120876275,-1.8357396455362,320.84171424425));
#10386=CARTESIAN_POINT('Ctrl Pts',(-31.8266553871769,-1.8357396455362,320.845304515018));
#10387=CARTESIAN_POINT('Ctrl Pts',(-31.834678941052,-1.8357396455362,320.848896219547));
#10388=CARTESIAN_POINT('Ctrl Pts',(-31.8383935430248,-1.8357396455362,320.850559042897));
#10389=CARTESIAN_POINT('Ctrl Pts',(-31.8421110078627,-1.8357396455362,320.852225347479));
#10390=CARTESIAN_POINT('Ctrl Pts',(-31.8458365934522,-1.8357396455362,320.853897526144));
#10391=CARTESIAN_POINT('Ctrl Pts',(-31.8943141308875,-1.8357396455362,320.875656012666));
#10392=CARTESIAN_POINT('Ctrl Pts',(-31.9438878817209,-1.8357396455362,320.898282844771));
#10393=CARTESIAN_POINT('Ctrl Pts',(-31.9945004898157,-1.8357396455362,320.921848711034));
#10394=CARTESIAN_POINT('Ctrl Pts',(-32.0435915780867,-1.83573964553619,
320.944706138548));
#10395=CARTESIAN_POINT('Ctrl Pts',(-32.0936601971404,-1.8357396455362,320.968447061434));
#10396=CARTESIAN_POINT('Ctrl Pts',(-32.1446063538921,-1.8357396455362,320.993131362249));
#10397=CARTESIAN_POINT('Ctrl Pts',(-32.1940839096517,-1.83573964553619,
321.01710410029));
#10398=CARTESIAN_POINT('Ctrl Pts',(-32.244389327626,-1.83573964553619,321.04196668715));
#10399=CARTESIAN_POINT('Ctrl Pts',(-32.2953825917274,-1.83573964553619,
321.06776848529));
#10400=CARTESIAN_POINT('Ctrl Pts',(-32.3464999294076,-1.83573964553619,
321.09363306273));
#10401=CARTESIAN_POINT('Ctrl Pts',(-32.3983089480635,-1.83573964553619,
321.120441552904));
#10402=CARTESIAN_POINT('Ctrl Pts',(-32.4506138713051,-1.83573964553619,
321.148236549717));
#10403=CARTESIAN_POINT('Ctrl Pts',(-32.4993675440086,-1.83573964553618,
321.17414440109));
#10404=CARTESIAN_POINT('Ctrl Pts',(-32.5485518829854,-1.83573964553618,
321.20090937913));
#10405=CARTESIAN_POINT('Ctrl Pts',(-32.5979598565244,-1.83573964553618,
321.228558830698));
#10406=CARTESIAN_POINT('Ctrl Pts',(-32.6463013406213,-1.83573964553618,
321.255611458594));
#10407=CARTESIAN_POINT('Ctrl Pts',(-32.6948571014369,-1.83573964553618,
321.283510876491));
#10408=CARTESIAN_POINT('Ctrl Pts',(-32.7433845017131,-1.83573964553617,
321.312274677328));
#10409=CARTESIAN_POINT('Ctrl Pts',(-32.7904668306801,-1.83573964553617,
321.340181936437));
#10410=CARTESIAN_POINT('Ctrl Pts',(-32.8375225714865,-1.83573964553617,
321.368902940896));
#10411=CARTESIAN_POINT('Ctrl Pts',(-32.8842816827013,-1.83573964553617,
321.39844495528));
#10412=CARTESIAN_POINT('Ctrl Pts',(-32.8986071664417,-1.83573964553617,
321.407495675787));
#10413=CARTESIAN_POINT('Ctrl Pts',(-32.9129044496341,-1.83573964553617,
321.416623388818));
#10414=CARTESIAN_POINT('Ctrl Pts',(-32.9271647914283,-1.83573964553617,
321.425828112808));
#10415=CARTESIAN_POINT('Ctrl Pts',(-32.9894393416746,-1.83573964553616,
321.466024908572));
#10416=CARTESIAN_POINT('Ctrl Pts',(-33.0508307284169,-1.83573964553616,
321.507320268099));
#10417=CARTESIAN_POINT('Ctrl Pts',(-33.1107858604198,-1.83573964553616,
321.549628247802));
#10418=CARTESIAN_POINT('Ctrl Pts',(-33.1720746579612,-1.83573964553616,
321.592877342846));
#10419=CARTESIAN_POINT('Ctrl Pts',(-33.2318608770518,-1.83573964553616,
321.63718525381));
#10420=CARTESIAN_POINT('Ctrl Pts',(-33.2895248559089,-1.83573964553616,
321.68241432941));
#10421=CARTESIAN_POINT('Ctrl Pts',(-33.3193726179928,-1.83573964553616,
321.705825594371));
#10422=CARTESIAN_POINT('Ctrl Pts',(-33.3486514607266,-1.83573964553616,
321.729482861706));
#10423=CARTESIAN_POINT('Ctrl Pts',(-33.3772752459844,-1.83573964553616,
321.753361462868));
#10424=CARTESIAN_POINT('Ctrl Pts',(-33.3842931760298,-1.83573964553616,
321.759215976903));
#10425=CARTESIAN_POINT('Ctrl Pts',(-33.391271734033,-1.83573964553616,321.765083776658));
#10426=CARTESIAN_POINT('Ctrl Pts',(-33.3982096632514,-1.83573964553616,
321.77096446054));
#10427=CARTESIAN_POINT('Ctrl Pts',(-33.402477062095,-1.83573964553616,321.774581566281));
#10428=CARTESIAN_POINT('Ctrl Pts',(-33.4067290901233,-1.83573964553616,
321.778203546127));
#10429=CARTESIAN_POINT('Ctrl Pts',(-33.4109654563272,-1.83573964553616,
321.781830303713));
#10430=CARTESIAN_POINT('Ctrl Pts',(-33.4148431507004,-1.83573964553616,
321.785150001966));
#10431=CARTESIAN_POINT('Ctrl Pts',(-33.4187026046589,-1.83573964553616,
321.788469247158));
#10432=CARTESIAN_POINT('Ctrl Pts',(-33.4225714468093,-1.83573964553616,
321.791812128747));
#10433=CARTESIAN_POINT('Ctrl Pts',(-33.4452246673039,-1.83573964553616,
321.811385693854));
#10434=CARTESIAN_POINT('Ctrl Pts',(-33.4680629603235,-1.83573964553616,
321.831651975973));
#10435=CARTESIAN_POINT('Ctrl Pts',(-33.4910161306369,-1.83573964553615,
321.852677020657));
#10436=CARTESIAN_POINT('Ctrl Pts',(-33.5136942685448,-1.83573964553615,
321.87345013637));
#10437=CARTESIAN_POINT('Ctrl Pts',(-33.536484452749,-1.83573964553614,321.894964144132));
#10438=CARTESIAN_POINT('Ctrl Pts',(-33.5592711467275,-1.83573964553614,
321.917262733865));
#10439=CARTESIAN_POINT('Ctrl Pts',(-33.5821431274893,-1.83573964553613,
321.939644783488));
#10440=CARTESIAN_POINT('Ctrl Pts',(-33.6050114507462,-1.83573964553612,
321.962817602908));
#10441=CARTESIAN_POINT('Ctrl Pts',(-33.6277123054661,-1.83573964553611,
321.98680122055));
#10442=CARTESIAN_POINT('Ctrl Pts',(-33.6506692348741,-1.8357396455361,322.011055382957));
#10443=CARTESIAN_POINT('Ctrl Pts',(-33.6734545419924,-1.8357396455361,322.03613915095));
#10444=CARTESIAN_POINT('Ctrl Pts',(-33.6958544071543,-1.83573964553609,
322.062043130631));
#10445=CARTESIAN_POINT('Ctrl Pts',(-33.7187953743038,-1.83573964553608,
322.088572859386));
#10446=CARTESIAN_POINT('Ctrl Pts',(-33.7413313269736,-1.83573964553607,
322.11596352265));
#10447=CARTESIAN_POINT('Ctrl Pts',(-33.7631941644085,-1.83573964553606,
322.144165673376));
#10448=CARTESIAN_POINT('Ctrl Pts',(-33.7848498866783,-1.83573964553606,
322.172100654155));
#10449=CARTESIAN_POINT('Ctrl Pts',(-33.8058437524814,-1.83573964553605,
322.200832290472));
#10450=CARTESIAN_POINT('Ctrl Pts',(-33.8258944208442,-1.83573964553605,
322.230266536138));
#10451=CARTESIAN_POINT('Ctrl Pts',(-33.8453345267723,-1.83573964553604,
322.258804480276));
#10452=CARTESIAN_POINT('Ctrl Pts',(-33.8638861983463,-1.83573964553604,
322.288003201187));
#10453=CARTESIAN_POINT('Ctrl Pts',(-33.8812971531608,-1.83573964553604,
322.317728145159));
#10454=CARTESIAN_POINT('Ctrl Pts',(-33.8842353512208,-1.83573964553604,
322.322744399215));
#10455=CARTESIAN_POINT('Ctrl Pts',(-33.8871411114321,-1.83573964553604,
322.327775517039));
#10456=CARTESIAN_POINT('Ctrl Pts',(-33.8900132952667,-1.83573964553604,
322.332820698899));
#10457=CARTESIAN_POINT('Ctrl Pts',(-33.8922620434555,-1.83573964553604,
322.336770774598));
#10458=CARTESIAN_POINT('Ctrl Pts',(-33.8944852638419,-1.83573964553604,
322.340720790062));
#10459=CARTESIAN_POINT('Ctrl Pts',(-33.8966822147502,-1.83573964553604,
322.344669336975));
#10460=CARTESIAN_POINT('Ctrl Pts',(-33.908306979514,-1.83573964553604,322.365562352312));
#10461=CARTESIAN_POINT('Ctrl Pts',(-33.9191931896151,-1.83573964553604,
322.386415387575));
#10462=CARTESIAN_POINT('Ctrl Pts',(-33.9292861005445,-1.83573964553604,
322.407067430352));
#10463=CARTESIAN_POINT('Ctrl Pts',(-33.9417031850838,-1.83573964553604,
322.432475180689));
#10464=CARTESIAN_POINT('Ctrl Pts',(-33.9535747838004,-1.83573964553603,
322.458172095153));
#10465=CARTESIAN_POINT('Ctrl Pts',(-33.9646867938464,-1.83573964553603,
322.48422003015));
#10466=CARTESIAN_POINT('Ctrl Pts',(-33.9758929094462,-1.83573964553603,
322.510488560281));
#10467=CARTESIAN_POINT('Ctrl Pts',(-33.9863256532958,-1.83573964553603,
322.537116716453));
#10468=CARTESIAN_POINT('Ctrl Pts',(-33.9958101702624,-1.83573964553603,
322.564189811733));
#10469=CARTESIAN_POINT('Ctrl Pts',(-34.0044657106833,-1.83573964553603,
322.588896633529));
#10470=CARTESIAN_POINT('Ctrl Pts',(-34.0123316649783,-1.83573964553602,
322.613975863777));
#10471=CARTESIAN_POINT('Ctrl Pts',(-34.0193159260718,-1.83573964553602,
322.639478830175));
#10472=CARTESIAN_POINT('Ctrl Pts',(-34.0257653553784,-1.83573964553602,
322.663028863126));
#10473=CARTESIAN_POINT('Ctrl Pts',(-34.0314631555427,-1.83573964553602,
322.686941105851));
#10474=CARTESIAN_POINT('Ctrl Pts',(-34.0363709590321,-1.83573964553602,
322.711226053297));
#10475=CARTESIAN_POINT('Ctrl Pts',(-34.041025494538,-1.83573964553602,322.734257772149));
#10476=CARTESIAN_POINT('Ctrl Pts',(-34.0449696036042,-1.83573964553602,
322.757625216962));
#10477=CARTESIAN_POINT('Ctrl Pts',(-34.0482003522234,-1.83573964553602,
322.781299822668));
#10478=CARTESIAN_POINT('Ctrl Pts',(-34.0501436708371,-1.83573964553602,
322.795540268882));
#10479=CARTESIAN_POINT('Ctrl Pts',(-34.0518290402368,-1.83573964553602,
322.809886093616));
#10480=CARTESIAN_POINT('Ctrl Pts',(-34.0532629695465,-1.83573964553602,
322.824344280636));
#10481=CARTESIAN_POINT('Ctrl Pts',(-34.0565952221417,-1.83573964553602,
322.857943099554));
#10482=CARTESIAN_POINT('Ctrl Pts',(-34.0585719809737,-1.83573964553602,
322.892167056002));
#10483=CARTESIAN_POINT('Ctrl Pts',(-34.0592900193062,-1.83573964553602,
322.927181258509));
#10484=CARTESIAN_POINT('Ctrl Pts',(-34.0600957471952,-1.83573964553602,
322.966471527839));
#10485=CARTESIAN_POINT('Ctrl Pts',(-34.0593169296225,-1.83573964553602,
323.006756557858));
#10486=CARTESIAN_POINT('Ctrl Pts',(-34.0570826346808,-1.83573964553602,
323.04820125649));
#10487=CARTESIAN_POINT('Ctrl Pts',(-34.0546549635249,-1.83573964553602,
323.093232956449));
#10488=CARTESIAN_POINT('Ctrl Pts',(-34.0505094908001,-1.83573964553602,
323.139632603362));
#10489=CARTESIAN_POINT('Ctrl Pts',(-34.0447957566754,-1.83573964553602,
323.187547675021));
#10490=CARTESIAN_POINT('Ctrl Pts',(-34.038259975017,-1.83573964553602,323.242356393747));
#10491=CARTESIAN_POINT('Ctrl Pts',(-34.0296733436094,-1.83573964553602,
323.299146247536));
#10492=CARTESIAN_POINT('Ctrl Pts',(-34.0192255510742,-1.83573964553602,
323.358080505269));
#10493=CARTESIAN_POINT('Ctrl Pts',(-34.0170778601807,-1.83573964553602,
323.370195271926));
#10494=CARTESIAN_POINT('Ctrl Pts',(-34.0148513871182,-1.83573964553602,
323.382400539659));
#10495=CARTESIAN_POINT('Ctrl Pts',(-34.0125475629435,-1.83573964553602,
323.394697592393));
#10496=CARTESIAN_POINT('Ctrl Pts',(-34.0041018612148,-1.83573964553602,
323.439777959496));
#10497=CARTESIAN_POINT('Ctrl Pts',(-33.9942378325614,-1.83573964553602,
323.485814537124));
#10498=CARTESIAN_POINT('Ctrl Pts',(-33.9830516029654,-1.83573964553602,
323.532667514042));
#10499=CARTESIAN_POINT('Ctrl Pts',(-33.9774997327527,-1.83573964553602,
323.555921251567));
#10500=CARTESIAN_POINT('Ctrl Pts',(-33.9716218371869,-1.83573964553602,
323.579376834424));
#10501=CARTESIAN_POINT('Ctrl Pts',(-33.9654276732709,-1.83573964553602,
323.603021343023));
#10502=CARTESIAN_POINT('Ctrl Pts',(-33.9632700493645,-1.83573964553602,
323.611257475889));
#10503=CARTESIAN_POINT('Ctrl Pts',(-33.9610740391173,-1.83573964553602,
323.619516555429));
#10504=CARTESIAN_POINT('Ctrl Pts',(-33.9588400165219,-1.83573964553602,
323.627798109298));
#10505=CARTESIAN_POINT('Ctrl Pts',(-33.9564896033297,-1.83573964553602,
323.636511124783));
#10506=CARTESIAN_POINT('Ctrl Pts',(-33.9540990870536,-1.83573964553602,
323.645241639339));
#10507=CARTESIAN_POINT('Ctrl Pts',(-33.9516709686306,-1.83573964553602,
323.65398245155));
#10508=CARTESIAN_POINT('Ctrl Pts',(-33.9357853389242,-1.83573964553602,
323.711168009224));
#10509=CARTESIAN_POINT('Ctrl Pts',(-33.9182697075581,-1.83573964553602,
323.768868124603));
#10510=CARTESIAN_POINT('Ctrl Pts',(-33.8993853314942,-1.83573964553602,
323.826715308049));
#10511=CARTESIAN_POINT('Ctrl Pts',(-33.8800632346799,-1.83573964553602,
323.885903330742));
#10512=CARTESIAN_POINT('Ctrl Pts',(-33.8593084218265,-1.83573964553602,
323.945245508614));
#10513=CARTESIAN_POINT('Ctrl Pts',(-33.8373921670454,-1.83573964553602,
324.004402817836));
#10514=CARTESIAN_POINT('Ctrl Pts',(-33.8149747048381,-1.83573964553602,
324.064913007967));
#10515=CARTESIAN_POINT('Ctrl Pts',(-33.7913422861375,-1.83573964553602,
324.125229980845));
#10516=CARTESIAN_POINT('Ctrl Pts',(-33.7667730232481,-1.83573964553602,
324.185044365047));
#10517=CARTESIAN_POINT('Ctrl Pts',(-33.7416528239998,-1.83573964553602,
324.246200015334));
#10518=CARTESIAN_POINT('Ctrl Pts',(-33.7155535047727,-1.83573964553602,
324.306830500987));
#10519=CARTESIAN_POINT('Ctrl Pts',(-33.688756410067,-1.83573964553602,324.366657164168));
#10520=CARTESIAN_POINT('Ctrl Pts',(-33.6610730441396,-1.83573964553602,
324.428462498934));
#10521=CARTESIAN_POINT('Ctrl Pts',(-33.6326452286528,-1.83573964553602,
324.489410106731));
#10522=CARTESIAN_POINT('Ctrl Pts',(-33.6037627924071,-1.83573964553602,
324.549244951856));
#10523=CARTESIAN_POINT('Ctrl Pts',(-33.5743135645162,-1.83573964553602,
324.610254001608));
#10524=CARTESIAN_POINT('Ctrl Pts',(-33.5443918862764,-1.83573964553602,
324.670106451295));
#10525=CARTESIAN_POINT('Ctrl Pts',(-33.5142808658538,-1.83573964553602,
324.728582005185));
#10526=CARTESIAN_POINT('Ctrl Pts',(-33.4835938597027,-1.83573964553602,
324.788176122446));
#10527=CARTESIAN_POINT('Ctrl Pts',(-33.4527103648113,-1.83573964553602,
324.846340431949));
#10528=CARTESIAN_POINT('Ctrl Pts',(-33.4219025092202,-1.83573964553602,
324.902889128396));
#10529=CARTESIAN_POINT('Ctrl Pts',(-33.3905174326719,-1.83573964553602,
324.960497330351));
#10530=CARTESIAN_POINT('Ctrl Pts',(-33.3592109971336,-1.83573964553602,
325.016429079736));
#10531=CARTESIAN_POINT('Ctrl Pts',(-33.3282402415969,-1.83573964553602,
325.070532506465));
#10532=CARTESIAN_POINT('Ctrl Pts',(-33.2964229457686,-1.83573964553602,
325.12611477121));
#10533=CARTESIAN_POINT('Ctrl Pts',(-33.2649600954318,-1.83573964553602,
325.179767610976));
#10534=CARTESIAN_POINT('Ctrl Pts',(-33.2340958895624,-1.83573964553602,
325.2313693393));
#10535=CARTESIAN_POINT('Ctrl Pts',(-33.2027399820095,-1.83573964553602,
325.28379314148));
#10536=CARTESIAN_POINT('Ctrl Pts',(-33.1720020130319,-1.83573964553602,
325.334100243464));
#10537=CARTESIAN_POINT('Ctrl Pts',(-33.1421012133259,-1.83573964553602,
325.382202871795));
#10538=CARTESIAN_POINT('Ctrl Pts',(-33.1115143190432,-1.83573964553602,
325.431409248278));
#10539=CARTESIAN_POINT('Ctrl Pts',(-33.0818035308545,-1.83573964553602,
325.478309060226));
#10540=CARTESIAN_POINT('Ctrl Pts',(-33.0531641026355,-1.83573964553602,
325.522845750499));
#10541=CARTESIAN_POINT('Ctrl Pts',(-33.0470426896219,-1.83573964553602,
325.532365056308));
#10542=CARTESIAN_POINT('Ctrl Pts',(-33.0409700794532,-1.83573964553602,
325.541776528307));
#10543=CARTESIAN_POINT('Ctrl Pts',(-33.0349479481876,-1.83573964553602,
325.551079813359));
#10544=CARTESIAN_POINT('Ctrl Pts',(16.317900533139,-13.,313.50573217442));
#10545=CARTESIAN_POINT('Ctrl Pts',(16.317900533139,9.8,313.50573217442));
#10546=CARTESIAN_POINT('Ctrl Pts',(15.6278893738391,-13.,313.517231811529));
#10547=CARTESIAN_POINT('Ctrl Pts',(15.6278893738391,9.8,313.517231811529));
#10548=CARTESIAN_POINT('Ctrl Pts',(14.2382065932492,-13.,313.544340068234));
#10549=CARTESIAN_POINT('Ctrl Pts',(14.2382065932492,9.8,313.544340068234));
#10550=CARTESIAN_POINT('Ctrl Pts',(12.1247011523636,-13.,313.597329370257));
#10551=CARTESIAN_POINT('Ctrl Pts',(12.1247011523636,9.8,313.597329370257));
#10552=CARTESIAN_POINT('Ctrl Pts',(9.24849377203438,-13.,313.692736456781));
#10553=CARTESIAN_POINT('Ctrl Pts',(9.24849377203438,9.8,313.692736456781));
#10554=CARTESIAN_POINT('Ctrl Pts',(5.55693877490966,-13.,313.853990642));
#10555=CARTESIAN_POINT('Ctrl Pts',(5.55693877490966,9.8,313.853990642));
#10556=CARTESIAN_POINT('Ctrl Pts',(1.77365151465576,-13.,314.058420030254));
#10557=CARTESIAN_POINT('Ctrl Pts',(1.77365151465576,9.8,314.058420030254));
#10558=CARTESIAN_POINT('Ctrl Pts',(-2.09023353797942,-13.,314.307572958727));
#10559=CARTESIAN_POINT('Ctrl Pts',(-2.09023353797942,9.8,314.307572958727));
#10560=CARTESIAN_POINT('Ctrl Pts',(-6.01421082656319,-13.,314.603269922693));
#10561=CARTESIAN_POINT('Ctrl Pts',(-6.01421082656319,9.8,314.603269922693));
#10562=CARTESIAN_POINT('Ctrl Pts',(-9.96528300844179,-13.,314.947459907816));
#10563=CARTESIAN_POINT('Ctrl Pts',(-9.96528300844179,9.8,314.947459907816));
#10564=CARTESIAN_POINT('Ctrl Pts',(-13.8949806972268,-13.,315.342078621379));
#10565=CARTESIAN_POINT('Ctrl Pts',(-13.8949806972268,9.8,315.342078621379));
#10566=CARTESIAN_POINT('Ctrl Pts',(-17.7352861120235,-13.,315.788771798629));
#10567=CARTESIAN_POINT('Ctrl Pts',(-17.7352861120235,9.8,315.788771798629));
#10568=CARTESIAN_POINT('Ctrl Pts',(-21.4049153651519,-13.,316.289764409719));
#10569=CARTESIAN_POINT('Ctrl Pts',(-21.4049153651519,9.8,316.289764409719));
#10570=CARTESIAN_POINT('Ctrl Pts',(-24.816789975018,-13.,316.848860723812));
#10571=CARTESIAN_POINT('Ctrl Pts',(-24.816789975018,9.8,316.848860723812));
#10572=CARTESIAN_POINT('Ctrl Pts',(-27.8849099804094,-13.,317.472300272892));
#10573=CARTESIAN_POINT('Ctrl Pts',(-27.8849099804094,9.8,317.472300272892));
#10574=CARTESIAN_POINT('Ctrl Pts',(-30.5321818074848,-13.,318.169788020995));
#10575=CARTESIAN_POINT('Ctrl Pts',(-30.5321818074848,9.8,318.169788020995));
#10576=CARTESIAN_POINT('Ctrl Pts',(-32.6972316847666,-13.,318.955110299069));
#10577=CARTESIAN_POINT('Ctrl Pts',(-32.6972316847666,9.8,318.955110299069));
#10578=CARTESIAN_POINT('Ctrl Pts',(-34.3449909415671,-13.,319.847716424401));
#10579=CARTESIAN_POINT('Ctrl Pts',(-34.3449909415671,9.8,319.847716424401));
#10580=CARTESIAN_POINT('Ctrl Pts',(-35.4659463455679,-13.,320.870731328741));
#10581=CARTESIAN_POINT('Ctrl Pts',(-35.4659463455679,9.8,320.870731328741));
#10582=CARTESIAN_POINT('Ctrl Pts',(-36.0649390676042,-13.,322.045906266434));
#10583=CARTESIAN_POINT('Ctrl Pts',(-36.0649390676042,9.8,322.045906266434));
#10584=CARTESIAN_POINT('Ctrl Pts',(-36.1525158245396,-13.,323.376843256979));
#10585=CARTESIAN_POINT('Ctrl Pts',(-36.1525158245396,9.8,323.376843256979));
#10586=CARTESIAN_POINT('Ctrl Pts',(-35.8309106944867,-13.,324.574753662996));
#10587=CARTESIAN_POINT('Ctrl Pts',(-35.8309106944867,9.8,324.574753662996));
#10588=CARTESIAN_POINT('Ctrl Pts',(-35.3753093664648,-13.,325.545731390974));
#10589=CARTESIAN_POINT('Ctrl Pts',(-35.3753093664648,9.8,325.545731390974));
#10590=CARTESIAN_POINT('Ctrl Pts',(-34.9799772611192,-13.,326.221291010618));
#10591=CARTESIAN_POINT('Ctrl Pts',(-34.9799772611192,9.8,326.221291010618));
#10592=CARTESIAN_POINT('Ctrl Pts',(-34.764378631884,-13.,326.559316446249));
#10593=CARTESIAN_POINT('Ctrl Pts',(-34.764378631884,9.8,326.559316446249));
#10594=CARTESIAN_POINT('',(-34.7643786318829,6.,326.55931644625));
#10595=CARTESIAN_POINT('',(-34.7643786318829,-13.,326.55931644625));
#10596=CARTESIAN_POINT('',(-20.0405545273386,6.,316.115431789383));
#10597=CARTESIAN_POINT('Ctrl Pts',(-20.0405545273386,6.,316.115431789383));
#10598=CARTESIAN_POINT('Ctrl Pts',(-20.3036630893018,6.,316.152450462513));
#10599=CARTESIAN_POINT('Ctrl Pts',(-21.2854516430835,6.,316.292780715073));
#10600=CARTESIAN_POINT('Ctrl Pts',(-22.949299720497,6.,316.545285451221));
#10601=CARTESIAN_POINT('Ctrl Pts',(-25.2075030604738,6.,316.92825331256));
#10602=CARTESIAN_POINT('Ctrl Pts',(-27.8849099804094,6.,317.472300272892));
#10603=CARTESIAN_POINT('Ctrl Pts',(-30.5321818074848,6.,318.169788020995));
#10604=CARTESIAN_POINT('Ctrl Pts',(-32.6972316847666,6.,318.955110299069));
#10605=CARTESIAN_POINT('Ctrl Pts',(-34.3449909415671,6.,319.847716424401));
#10606=CARTESIAN_POINT('Ctrl Pts',(-35.4659463455679,6.,320.870731328741));
#10607=CARTESIAN_POINT('Ctrl Pts',(-36.0649390676042,6.,322.045906266434));
#10608=CARTESIAN_POINT('Ctrl Pts',(-36.1525158245396,6.,323.376843256979));
#10609=CARTESIAN_POINT('Ctrl Pts',(-35.8309106944867,6.,324.574753662996));
#10610=CARTESIAN_POINT('Ctrl Pts',(-35.3753093664648,6.,325.545731390973));
#10611=CARTESIAN_POINT('Ctrl Pts',(-34.9799772611192,6.,326.221291010618));
#10612=CARTESIAN_POINT('Ctrl Pts',(-34.764378631884,6.,326.559316446249));
#10613=CARTESIAN_POINT('',(16.317900533139,6.,313.50573217442));
#10614=CARTESIAN_POINT('Ctrl Pts',(16.317900533139,6.,313.50573217442));
#10615=CARTESIAN_POINT('Ctrl Pts',(15.6278893738391,6.,313.517231811529));
#10616=CARTESIAN_POINT('Ctrl Pts',(14.2382065932492,6.,313.544340068234));
#10617=CARTESIAN_POINT('Ctrl Pts',(12.1247011523636,6.,313.597329370257));
#10618=CARTESIAN_POINT('Ctrl Pts',(9.24849377203438,6.,313.692736456781));
#10619=CARTESIAN_POINT('Ctrl Pts',(5.55693877490966,6.,313.853990642));
#10620=CARTESIAN_POINT('Ctrl Pts',(1.77365151465576,6.,314.058420030254));
#10621=CARTESIAN_POINT('Ctrl Pts',(-2.09023353797942,6.,314.307572958727));
#10622=CARTESIAN_POINT('Ctrl Pts',(-6.01421082656319,6.,314.603269922693));
#10623=CARTESIAN_POINT('Ctrl Pts',(-9.96528300844179,6.,314.947459907816));
#10624=CARTESIAN_POINT('Ctrl Pts',(-13.6094727938912,6.,315.313408028766));
#10625=CARTESIAN_POINT('Ctrl Pts',(-16.408608787372,6.,315.634868750851));
#10626=CARTESIAN_POINT('Ctrl Pts',(-18.3821515018489,6.,315.886718461855));
#10627=CARTESIAN_POINT('Ctrl Pts',(-19.579383939224,6.,316.050546317275));
#10628=CARTESIAN_POINT('Ctrl Pts',(-20.0405545273386,6.,316.115431789383));
#10629=CARTESIAN_POINT('',(16.317900533139,-6.,313.50573217442));
#10630=CARTESIAN_POINT('',(16.317900533139,-13.,313.50573217442));
#10631=CARTESIAN_POINT('',(-20.0405545265874,-6.,316.115431789172));
#10632=CARTESIAN_POINT('Ctrl Pts',(-20.0405545265728,-6.,316.115431789276));
#10633=CARTESIAN_POINT('Ctrl Pts',(-19.4004600929468,-6.,316.025372209181));
#10634=CARTESIAN_POINT('Ctrl Pts',(-18.7497721478954,-6.,315.937974131023));
#10635=CARTESIAN_POINT('Ctrl Pts',(-18.0906230620982,-6.00000000000001,
315.853146441753));
#10636=CARTESIAN_POINT('Ctrl Pts',(-17.5243686223842,-6.00000000000001,
315.780273617235));
#10637=CARTESIAN_POINT('Ctrl Pts',(-16.9518707527639,-6.00000000000001,
315.709298340212));
#10638=CARTESIAN_POINT('Ctrl Pts',(-16.3744431251552,-6.00000000000001,
315.640175937909));
#10639=CARTESIAN_POINT('Ctrl Pts',(-15.8474128379684,-6.00000000000001,
315.577086473887));
#10640=CARTESIAN_POINT('Ctrl Pts',(-15.3162762637607,-6.00000000000002,
315.515540826831));
#10641=CARTESIAN_POINT('Ctrl Pts',(-14.7819888683864,-6.00000000000002,
315.455511511763));
#10642=CARTESIAN_POINT('Ctrl Pts',(-14.2794448395025,-6.00000000000002,
315.399048690243));
#10643=CARTESIAN_POINT('Ctrl Pts',(-13.7741136098437,-6.00000000000002,
315.34392752094));
#10644=CARTESIAN_POINT('Ctrl Pts',(-13.2667442133851,-6.00000000000002,
315.290128438354));
#10645=CARTESIAN_POINT('Ctrl Pts',(-12.7800008415808,-6.00000000000002,
315.238516443147));
#10646=CARTESIAN_POINT('Ctrl Pts',(-12.2913818748689,-6.00000000000002,
315.188121314751));
#10647=CARTESIAN_POINT('Ctrl Pts',(-11.8015007656218,-6.00000000000003,
315.138927292701));
#10648=CARTESIAN_POINT('Ctrl Pts',(-11.3278770637046,-6.00000000000003,
315.09136584484));
#10649=CARTESIAN_POINT('Ctrl Pts',(-10.8530737841221,-6.00000000000003,
315.04492717112));
#10650=CARTESIAN_POINT('Ctrl Pts',(-10.3775966580326,-6.00000000000003,
314.999597383367));
#10651=CARTESIAN_POINT('Ctrl Pts',(-9.90819256207086,-6.00000000000003,
314.954846570189));
#10652=CARTESIAN_POINT('Ctrl Pts',(-9.43813190999691,-6.00000000000004,
314.91117654094));
#10653=CARTESIAN_POINT('Ctrl Pts',(-8.96784969603263,-6.00000000000004,
314.868573440465));
#10654=CARTESIAN_POINT('Ctrl Pts',(-8.48876740980112,-6.00000000000004,
314.825173137051));
#10655=CARTESIAN_POINT('Ctrl Pts',(-8.00945507896517,-6.00000000000004,
314.782880048696));
#10656=CARTESIAN_POINT('Ctrl Pts',(-7.53031845791347,-6.00000000000004,
314.74167888733));
#10657=CARTESIAN_POINT('Ctrl Pts',(-7.04087742046235,-6.00000000000004,
314.699591644826));
#10658=CARTESIAN_POINT('Ctrl Pts',(-6.55161960647171,-6.00000000000004,
314.658643780709));
#10659=CARTESIAN_POINT('Ctrl Pts',(-6.06292338188131,-6.00000000000005,
314.61881862178));
#10660=CARTESIAN_POINT('Ctrl Pts',(-5.55931863250807,-6.00000000000005,
314.577778527398));
#10661=CARTESIAN_POINT('Ctrl Pts',(-5.05631021845046,-6.00000000000005,
314.53793066474));
#10662=CARTESIAN_POINT('Ctrl Pts',(-4.5542566466415,-6.00000000000005,314.499256707419));
#10663=CARTESIAN_POINT('Ctrl Pts',(-4.04238010851235,-6.00000000000005,
314.459826071923));
#10664=CARTESIAN_POINT('Ctrl Pts',(-3.5314960243371,-6.00000000000005,314.42161571284));
#10665=CARTESIAN_POINT('Ctrl Pts',(-3.0219286923217,-6.00000000000006,314.384606361902));
#10666=CARTESIAN_POINT('Ctrl Pts',(-2.50115143391243,-6.00000000000006,
314.346782845546));
#10667=CARTESIAN_POINT('Ctrl Pts',(-1.98174936982304,-6.00000000000006,
314.310213743213));
#10668=CARTESIAN_POINT('Ctrl Pts',(-1.46401295479278,-6.00000000000006,
314.274878890499));
#10669=CARTESIAN_POINT('Ctrl Pts',(-0.933109127184629,-6.00000000000006,
314.238645378602));
#10670=CARTESIAN_POINT('Ctrl Pts',(-0.403956593770315,-6.00000000000006,
314.203709674355));
#10671=CARTESIAN_POINT('Ctrl Pts',(0.123187284072103,-6.00000000000006,
314.170050747481));
#10672=CARTESIAN_POINT('Ctrl Pts',(0.665680905887875,-6.00000000000007,
314.135411716443));
#10673=CARTESIAN_POINT('Ctrl Pts',(1.20604737288525,-6.00000000000007,314.102124875805));
#10674=CARTESIAN_POINT('Ctrl Pts',(1.74406199402793,-6.00000000000007,314.070168409682));
#10675=CARTESIAN_POINT('Ctrl Pts',(2.29915491822338,-6.00000000000007,314.037197543222));
#10676=CARTESIAN_POINT('Ctrl Pts',(2.85174452453734,-6.00000000000007,314.00564282438));
#10677=CARTESIAN_POINT('Ctrl Pts',(3.40163952961782,-6.00000000000008,313.975481885011));
#10678=CARTESIAN_POINT('Ctrl Pts',(3.98358848909718,-6.00000000000008,313.943562832973));
#10679=CARTESIAN_POINT('Ctrl Pts',(4.56251959828842,-6.00000000000008,313.913204744328));
#10680=CARTESIAN_POINT('Ctrl Pts',(5.13826572536412,-6.00000000000008,313.884383410908));
#10681=CARTESIAN_POINT('Ctrl Pts',(5.73956593775672,-6.00000000000008,313.854282862954));
#10682=CARTESIAN_POINT('Ctrl Pts',(6.33739249073037,-6.00000000000009,313.8258584665));
#10683=CARTESIAN_POINT('Ctrl Pts',(6.93161508868178,-6.00000000000009,313.799085785577));
#10684=CARTESIAN_POINT('Ctrl Pts',(7.55902819791957,-6.00000000000009,313.770817707187));
#10685=CARTESIAN_POINT('Ctrl Pts',(8.18242392403445,-6.00000000000009,313.744390948001));
#10686=CARTESIAN_POINT('Ctrl Pts',(8.80170884735432,-6.00000000000009,313.71978104624));
#10687=CARTESIAN_POINT('Ctrl Pts',(9.50347615746683,-6.0000000000001,313.691893358505));
#10688=CARTESIAN_POINT('Ctrl Pts',(10.1999648801093,-6.0000000000001,313.666338546755));
#10689=CARTESIAN_POINT('Ctrl Pts',(10.8911103594156,-6.0000000000001,313.643088515844));
#10690=CARTESIAN_POINT('Ctrl Pts',(11.670124147706,-6.0000000000001,313.616882608115));
#10691=CARTESIAN_POINT('Ctrl Pts',(12.44235109068,-6.00000000000011,313.593604477312));
#10692=CARTESIAN_POINT('Ctrl Pts',(13.2077719903083,-6.00000000000011,313.573226843001));
#10693=CARTESIAN_POINT('Ctrl Pts',(14.2572610604321,-6.00000000000011,313.545286523506));
#10694=CARTESIAN_POINT('Ctrl Pts',(15.2939614463516,-6.00000000000012,313.522797011359));
#10695=CARTESIAN_POINT('Ctrl Pts',(16.317900533139,-6.00000000000012,313.50573217442));
#10696=CARTESIAN_POINT('',(-34.7643786318829,-6.,326.55931644625));
#10697=CARTESIAN_POINT('Ctrl Pts',(-20.0405545265728,-6.,316.115431789276));
#10698=CARTESIAN_POINT('Ctrl Pts',(-20.7549729434527,-6.,316.21594855564));
#10699=CARTESIAN_POINT('Ctrl Pts',(-21.4561906038213,-6.,316.319779472749));
#10700=CARTESIAN_POINT('Ctrl Pts',(-22.1412177785273,-6.,316.427092714018));
#10701=CARTESIAN_POINT('Ctrl Pts',(-22.6934545573852,-6.,316.513603615885));
#10702=CARTESIAN_POINT('Ctrl Pts',(-23.2351674585656,-6.,316.602378254545));
#10703=CARTESIAN_POINT('Ctrl Pts',(-23.7648154461404,-6.,316.693530260689));
#10704=CARTESIAN_POINT('Ctrl Pts',(-24.2381920307505,-6.,316.77499800221));
#10705=CARTESIAN_POINT('Ctrl Pts',(-24.7019304370803,-6.,316.858364961178));
#10706=CARTESIAN_POINT('Ctrl Pts',(-25.1549683114691,-6.,316.943730630041));
#10707=CARTESIAN_POINT('Ctrl Pts',(-25.5795553714899,-6.,317.023735328143));
#10708=CARTESIAN_POINT('Ctrl Pts',(-25.9947432901691,-6.,317.10549566778));
#10709=CARTESIAN_POINT('Ctrl Pts',(-26.3997003202801,-6.,317.189109078339));
#10710=CARTESIAN_POINT('Ctrl Pts',(-26.7856515095121,-6.,317.268798262232));
#10711=CARTESIAN_POINT('Ctrl Pts',(-27.1623093224257,-6.,317.350170711296));
#10712=CARTESIAN_POINT('Ctrl Pts',(-27.5289986025995,-6.,317.433324389979));
#10713=CARTESIAN_POINT('Ctrl Pts',(-27.8785558810865,-6.,317.512593065636));
#10714=CARTESIAN_POINT('Ctrl Pts',(-28.2190541342782,-6.,317.593480454025));
#10715=CARTESIAN_POINT('Ctrl Pts',(-28.5499534894729,-6.,317.676083421344));
#10716=CARTESIAN_POINT('Ctrl Pts',(-28.8655920291323,-6.,317.754876805395));
#10717=CARTESIAN_POINT('Ctrl Pts',(-29.1724963802546,-6.,317.835231170493));
#10718=CARTESIAN_POINT('Ctrl Pts',(-29.4702436223019,-6.,317.917241665508));
#10719=CARTESIAN_POINT('Ctrl Pts',(-29.7569275835638,-6.,317.996204927819));
#10720=CARTESIAN_POINT('Ctrl Pts',(-30.035122074916,-6.,318.076703525759));
#10721=CARTESIAN_POINT('Ctrl Pts',(-30.304496360236,-6.,318.158833019446));
#10722=CARTESIAN_POINT('Ctrl Pts',(-30.5702374847235,-6.,318.239854799161));
#10723=CARTESIAN_POINT('Ctrl Pts',(-30.8273945384287,-6.,318.322463785503));
#10724=CARTESIAN_POINT('Ctrl Pts',(-31.0757000696003,-6.,318.406762502099));
#10725=CARTESIAN_POINT('Ctrl Pts',(-31.324823150672,-6.,318.491338773558));
#10726=CARTESIAN_POINT('Ctrl Pts',(-31.5650363297957,-6.,318.577616001022));
#10727=CARTESIAN_POINT('Ctrl Pts',(-31.7961210268803,-6.,318.665707788871));
#10728=CARTESIAN_POINT('Ctrl Pts',(-32.0279623515194,-6.,318.754088010679));
#10729=CARTESIAN_POINT('Ctrl Pts',(-32.2506153233891,-6.,318.844294777607));
#10730=CARTESIAN_POINT('Ctrl Pts',(-32.4639109145767,-6.,318.936451698723));
#10731=CARTESIAN_POINT('Ctrl Pts',(-32.6810137977926,-6.,319.030253606071));
#10732=CARTESIAN_POINT('Ctrl Pts',(-32.888422294495,-6.,319.126076024321));
#10733=CARTESIAN_POINT('Ctrl Pts',(-33.0860121094894,-6.,319.224057177318));
#10734=CARTESIAN_POINT('Ctrl Pts',(-33.297622908898,-6.,319.328991078457));
#10735=CARTESIAN_POINT('Ctrl Pts',(-33.4979721328517,-6.,319.436401195976));
#10736=CARTESIAN_POINT('Ctrl Pts',(-33.6869681337662,-6.,319.546463366874));
#10737=CARTESIAN_POINT('Ctrl Pts',(-33.8864368406078,-6.,319.662624337449));
#10738=CARTESIAN_POINT('Ctrl Pts',(-34.0732596226775,-6.,319.78173982131));
#10739=CARTESIAN_POINT('Ctrl Pts',(-34.2473912238251,-6.,319.90401788643));
#10740=CARTESIAN_POINT('Ctrl Pts',(-34.4306171129455,-6.,320.03268210966));
#10741=CARTESIAN_POINT('Ctrl Pts',(-34.5997920592249,-6.,320.164848461445));
#10742=CARTESIAN_POINT('Ctrl Pts',(-34.7549231941343,-6.,320.300752983988));
#10743=CARTESIAN_POINT('Ctrl Pts',(-34.9175912336802,-6.,320.443260303749));
#10744=CARTESIAN_POINT('Ctrl Pts',(-35.0648183398604,-6.,320.589878647392));
#10745=CARTESIAN_POINT('Ctrl Pts',(-35.1966684463826,-6.,320.740862499649));
#10746=CARTESIAN_POINT('Ctrl Pts',(-35.3331200653272,-6.,320.897115623886));
#10747=CARTESIAN_POINT('Ctrl Pts',(-35.4531036891042,-6.,321.058045238222));
#10748=CARTESIAN_POINT('Ctrl Pts',(-35.5567351883284,-6.,321.223901152682));
#10749=CARTESIAN_POINT('Ctrl Pts',(-35.666164567533,-6.,321.39903622158));
#10750=CARTESIAN_POINT('Ctrl Pts',(-35.7573622522126,-6.,321.579665476576));
#10751=CARTESIAN_POINT('Ctrl Pts',(-35.83049571681,-6.,321.766030282812));
#10752=CARTESIAN_POINT('Ctrl Pts',(-35.8990144606402,-6.,321.940635471939));
#10753=CARTESIAN_POINT('Ctrl Pts',(-35.9516781792488,-6.,322.120275264076));
#10754=CARTESIAN_POINT('Ctrl Pts',(-35.9886301568112,-6.,322.305095435263));
#10755=CARTESIAN_POINT('Ctrl Pts',(-36.0272612985265,-6.,322.498314166599));
#10756=CARTESIAN_POINT('Ctrl Pts',(-36.0487207806161,-6.,322.697194451537));
#10757=CARTESIAN_POINT('Ctrl Pts',(-36.0531635744342,-6.,322.901842878652));
#10758=CARTESIAN_POINT('Ctrl Pts',(-36.0578748107463,-6.,323.1188565733));
#10759=CARTESIAN_POINT('Ctrl Pts',(-36.0434514023682,-6.,323.342355832864));
#10760=CARTESIAN_POINT('Ctrl Pts',(-36.0100610340838,-6.,323.572410184283));
#10761=CARTESIAN_POINT('Ctrl Pts',(-35.9748650024435,-6.,323.814905270369));
#10762=CARTESIAN_POINT('Ctrl Pts',(-35.9185960651917,-6.,324.064682754654));
#10763=CARTESIAN_POINT('Ctrl Pts',(-35.8414212830246,-6.,324.321774846627));
#10764=CARTESIAN_POINT('Ctrl Pts',(-35.7641383003919,-6.,324.579227386447));
#10765=CARTESIAN_POINT('Ctrl Pts',(-35.6658915658653,-6.,324.844013841787));
#10766=CARTESIAN_POINT('Ctrl Pts',(-35.5468077850159,-6.,325.1161343829));
#10767=CARTESIAN_POINT('Ctrl Pts',(-35.4304704895933,-6.,325.381978879573));
#10768=CARTESIAN_POINT('Ctrl Pts',(-35.2942465138308,-6.,325.654821759961));
#10769=CARTESIAN_POINT('Ctrl Pts',(-35.1382069832313,-6.,325.934651028931));
#10770=CARTESIAN_POINT('Ctrl Pts',(-35.0241772447393,-6.,326.139143174226));
#10771=CARTESIAN_POINT('Ctrl Pts',(-34.8995644267643,-6.,326.347365946528));
#10772=CARTESIAN_POINT('Ctrl Pts',(-34.764378631884,-6.,326.559316446249));
#10773=CARTESIAN_POINT('',(-34.7643786318829,-13.,326.55931644625));
#10774=CARTESIAN_POINT('Origin',(-34.7643786318829,-13.,326.55931644625));
#10775=CARTESIAN_POINT('',(-33.0349479481876,6.,325.551079813359));
#10776=CARTESIAN_POINT('',(-33.0349479481876,-13.,325.551079813359));
#10777=CARTESIAN_POINT('',(-33.0349479481876,6.,325.551079813359));
#10778=CARTESIAN_POINT('Origin',(-9.91234501254369,-6.,320.032524310335));
#10779=CARTESIAN_POINT('',(-20.0407500733448,-6.,318.135777164329));
#10780=CARTESIAN_POINT('',(-20.0405545273386,-6.,325.214166745933));
#10781=CARTESIAN_POINT('',(-33.0349479481876,-6.,325.551079813359));
#10782=CARTESIAN_POINT('Ctrl Pts',(-33.0349479481876,-6.,325.551079813359));
#10783=CARTESIAN_POINT('Ctrl Pts',(-33.6174796157523,-6.,324.651156195591));
#10784=CARTESIAN_POINT('Ctrl Pts',(-33.9167172498653,-6.,323.906208160949));
#10785=CARTESIAN_POINT('Ctrl Pts',(-34.1037191682109,-6.,322.90805366785));
#10786=CARTESIAN_POINT('Ctrl Pts',(-34.0551194507184,-6.,322.664546739217));
#10787=CARTESIAN_POINT('Ctrl Pts',(-33.8035173417139,-6.,322.149720287837));
#10788=CARTESIAN_POINT('Ctrl Pts',(-33.5337647985207,-6.,321.817374523001));
#10789=CARTESIAN_POINT('Ctrl Pts',(-32.1374388202749,-6.,320.916078087379));
#10790=CARTESIAN_POINT('Ctrl Pts',(-30.8059455281908,-6.,320.365993587133));
#10791=CARTESIAN_POINT('Ctrl Pts',(-26.6717920677378,-6.,319.212778873305));
#10792=CARTESIAN_POINT('Ctrl Pts',(-23.5366870472917,-6.,318.635027950995));
#10793=CARTESIAN_POINT('Ctrl Pts',(-20.040945619351,-6.,318.135786350546));
#10794=CARTESIAN_POINT('',(-24.0704398622791,-6.,320.324882814963));
#10795=CARTESIAN_POINT('Ctrl Pts',(-33.0349479481876,-13.,325.551079813359));
#10796=CARTESIAN_POINT('Ctrl Pts',(-33.0349479481876,9.8,325.551079813359));
#10797=CARTESIAN_POINT('Ctrl Pts',(-33.6174796157523,-13.,324.651156195591));
#10798=CARTESIAN_POINT('Ctrl Pts',(-33.6174796157523,9.8,324.651156195591));
#10799=CARTESIAN_POINT('Ctrl Pts',(-33.9167172498653,-13.,323.906208160949));
#10800=CARTESIAN_POINT('Ctrl Pts',(-33.9167172498653,9.8,323.906208160949));
#10801=CARTESIAN_POINT('Ctrl Pts',(-34.0125475629435,-13.,323.394697592393));
#10802=CARTESIAN_POINT('Ctrl Pts',(-34.0125475629435,9.8,323.394697592393));
#10803=CARTESIAN_POINT('Ctrl Pts',(-34.1037191682109,-13.,322.90805366785));
#10804=CARTESIAN_POINT('Ctrl Pts',(-34.1037191682109,9.8,322.90805366785));
#10805=CARTESIAN_POINT('Ctrl Pts',(-34.0551194507184,-13.,322.664546739217));
#10806=CARTESIAN_POINT('Ctrl Pts',(-34.0551194507184,9.8,322.664546739217));
#10807=CARTESIAN_POINT('Ctrl Pts',(-33.9292861005445,-13.,322.407067430352));
#10808=CARTESIAN_POINT('Ctrl Pts',(-33.9292861005445,9.8,322.407067430352));
#10809=CARTESIAN_POINT('Ctrl Pts',(-33.8035173417139,-13.,322.149720287837));
#10810=CARTESIAN_POINT('Ctrl Pts',(-33.8035173417139,9.8,322.149720287837));
#10811=CARTESIAN_POINT('Ctrl Pts',(-33.5337647985207,-13.,321.817374523001));
#10812=CARTESIAN_POINT('Ctrl Pts',(-33.5337647985207,9.8,321.817374523001));
#10813=CARTESIAN_POINT('Ctrl Pts',(-32.9271647914283,-13.,321.425828112808));
#10814=CARTESIAN_POINT('Ctrl Pts',(-32.9271647914283,9.8,321.425828112808));
#10815=CARTESIAN_POINT('Ctrl Pts',(-32.1374388202749,-13.,320.916078087379));
#10816=CARTESIAN_POINT('Ctrl Pts',(-32.1374388202749,9.8,320.916078087379));
#10817=CARTESIAN_POINT('Ctrl Pts',(-30.8059455281908,-13.,320.365993587133));
#10818=CARTESIAN_POINT('Ctrl Pts',(-30.8059455281908,9.8,320.365993587133));
#10819=CARTESIAN_POINT('Ctrl Pts',(-29.043009016516,-13.,319.874225600227));
#10820=CARTESIAN_POINT('Ctrl Pts',(-29.043009016516,9.8,319.874225600227));
#10821=CARTESIAN_POINT('Ctrl Pts',(-25.8730053780895,-13.,318.989958754863));
#10822=CARTESIAN_POINT('Ctrl Pts',(-25.8730053780895,9.8,318.989958754863));
#10823=CARTESIAN_POINT('Ctrl Pts',(-21.3377690810308,-13.,318.255274354999));
#10824=CARTESIAN_POINT('Ctrl Pts',(-21.3377690810308,9.8,318.255274354999));
#10825=CARTESIAN_POINT('Ctrl Pts',(-16.4007776292659,-13.,317.65778048784));
#10826=CARTESIAN_POINT('Ctrl Pts',(-16.4007776292659,9.8,317.65778048784));
#10827=CARTESIAN_POINT('Ctrl Pts',(-11.7424615555448,-13.,317.094012996539));
#10828=CARTESIAN_POINT('Ctrl Pts',(-11.7424615555448,9.8,317.094012996539));
#10829=CARTESIAN_POINT('Ctrl Pts',(-6.76571504745064,-13.,316.650544330241));
#10830=CARTESIAN_POINT('Ctrl Pts',(-6.76571504745064,9.8,316.650544330241));
#10831=CARTESIAN_POINT('Ctrl Pts',(-1.96541115088432,-13.,316.314322154425));
#10832=CARTESIAN_POINT('Ctrl Pts',(-1.96541115088432,9.8,316.314322154425));
#10833=CARTESIAN_POINT('Ctrl Pts',(4.47207810420708,-13.,315.86342848378));
#10834=CARTESIAN_POINT('Ctrl Pts',(4.47207810420708,9.8,315.86342848378));
#10835=CARTESIAN_POINT('Ctrl Pts',(10.6153256845702,-13.,315.601684449612));
#10836=CARTESIAN_POINT('Ctrl Pts',(10.6153256845702,9.8,315.601684449612));
#10837=CARTESIAN_POINT('Ctrl Pts',(16.3179005331389,-13.,315.506011760182));
#10838=CARTESIAN_POINT('Ctrl Pts',(16.3179005331389,9.8,315.506011760182));
#10839=CARTESIAN_POINT('',(-33.0349479481876,-13.,325.551079813359));
#10840=CARTESIAN_POINT('',(16.3179005331391,-6.,315.506011760182));
#10841=CARTESIAN_POINT('Ctrl Pts',(16.3179005331389,-6.00000000000013,315.506011760182));
#10842=CARTESIAN_POINT('Ctrl Pts',(10.6153256845702,-6.00000000000013,315.601684449612));
#10843=CARTESIAN_POINT('Ctrl Pts',(4.47207810420708,-6.00000000000014,315.86342848378));
#10844=CARTESIAN_POINT('Ctrl Pts',(-6.76571504745064,-6.00000000000014,
316.650544330241));
#10845=CARTESIAN_POINT('Ctrl Pts',(-11.7424615555448,-6.00000000000014,
317.094012996539));
#10846=CARTESIAN_POINT('Ctrl Pts',(-17.6447244400945,-6.00000000000013,
317.808327758947));
#10847=CARTESIAN_POINT('Ctrl Pts',(-18.8631653699184,-6.00000000000013,
317.967584726398));
#10848=CARTESIAN_POINT('Ctrl Pts',(-20.0406883873031,-6.00000000000013,
318.135749614386));
#10849=CARTESIAN_POINT('',(16.3179005331391,6.,315.506011760182));
#10850=CARTESIAN_POINT('',(16.3179005331391,-13.,315.506011760182));
#10851=CARTESIAN_POINT('',(-20.0407500724488,6.00000000000001,318.135777164115));
#10852=CARTESIAN_POINT('Ctrl Pts',(-20.0406883866898,6.00000000000001,318.135749614298));
#10853=CARTESIAN_POINT('Ctrl Pts',(-18.8631653694953,6.00000000000001,317.967584726343));
#10854=CARTESIAN_POINT('Ctrl Pts',(-17.6447244398786,6.00000000000001,317.808327758921));
#10855=CARTESIAN_POINT('Ctrl Pts',(-11.7424615555448,6.00000000000001,317.094012996539));
#10856=CARTESIAN_POINT('Ctrl Pts',(-6.76571504745064,6.00000000000001,316.650544330241));
#10857=CARTESIAN_POINT('Ctrl Pts',(4.4720781042072,6.,315.86342848378));
#10858=CARTESIAN_POINT('Ctrl Pts',(10.6153256845705,6.,315.601684449612));
#10859=CARTESIAN_POINT('Ctrl Pts',(16.3179005331392,6.,315.506011760182));
#10860=CARTESIAN_POINT('Ctrl Pts',(-33.0349479481876,6.,325.551079813359));
#10861=CARTESIAN_POINT('Ctrl Pts',(-33.6174796157523,6.,324.651156195591));
#10862=CARTESIAN_POINT('Ctrl Pts',(-33.9167172498653,6.,323.906208160949));
#10863=CARTESIAN_POINT('Ctrl Pts',(-34.1037191682109,6.,322.90805366785));
#10864=CARTESIAN_POINT('Ctrl Pts',(-34.0551194507184,6.00000000000001,322.664546739217));
#10865=CARTESIAN_POINT('Ctrl Pts',(-33.8035173417139,6.00000000000001,322.149720287837));
#10866=CARTESIAN_POINT('Ctrl Pts',(-33.5337647985207,6.00000000000001,321.817374523001));
#10867=CARTESIAN_POINT('Ctrl Pts',(-32.1374388202749,6.00000000000001,320.916078087379));
#10868=CARTESIAN_POINT('Ctrl Pts',(-30.8059455281908,6.00000000000001,320.365993587133));
#10869=CARTESIAN_POINT('Ctrl Pts',(-26.6717920673326,6.00000000000001,319.212778873192));
#10870=CARTESIAN_POINT('Ctrl Pts',(-23.5366870462203,6.00000000000001,318.635027950798));
#10871=CARTESIAN_POINT('Ctrl Pts',(-20.0409456175589,6.00000000000001,318.13578635029));
#10872=CARTESIAN_POINT('Origin',(-34.7643786318829,-13.,326.55931644625));
#10873=CARTESIAN_POINT('Origin',(-9.91234501254369,6.,320.032524310335));
#10874=CARTESIAN_POINT('',(-20.0405545273386,6.,325.214166745933));
#10875=CARTESIAN_POINT('Origin',(-2.11984264684888,6.,322.999388292511));
#10876=CARTESIAN_POINT('',(16.317900533139,6.,326.637882383191));
#10877=CARTESIAN_POINT('',(16.317900533139,6.,315.999694146255));
#10878=CARTESIAN_POINT('',(-2.1198426468477,6.,336.998776585022));
#10879=CARTESIAN_POINT('Origin',(-2.35185291019846,6.,315.));
#10880=CARTESIAN_POINT('',(-20.0405545273386,6.,327.428945199355));
#10881=CARTESIAN_POINT('Origin',(-1.88783238349926,6.,315.));
#10882=CARTESIAN_POINT('',(-20.0405545273386,6.,325.214166745933));
#10883=CARTESIAN_POINT('',(-5.88783238349923,6.,328.556349186104));
#10884=CARTESIAN_POINT('Origin',(-1.88783238349926,6.,328.556349186104));
#10885=CARTESIAN_POINT('Origin',(-2.11984264684888,6.,322.999388292511));
#10886=CARTESIAN_POINT('',(-20.0405545273386,6.,325.214166745933));
#10887=CARTESIAN_POINT('',(16.317900533139,6.,315.999694146255));
#10888=CARTESIAN_POINT('Origin',(-20.0405545273386,-22.,327.428945199355));
#10889=CARTESIAN_POINT('',(-20.0405545273386,8.,327.428945199355));
#10890=CARTESIAN_POINT('',(-20.0405545273386,6.,327.428945199355));
#10891=CARTESIAN_POINT('',(-20.0405545273386,8.,325.214166745933));
#10892=CARTESIAN_POINT('Origin',(-2.11984264684888,8.,322.999388292511));
#10893=CARTESIAN_POINT('',(16.317900533139,8.,326.637882383191));
#10894=CARTESIAN_POINT('',(16.317900533139,8.,315.999694146255));
#10895=CARTESIAN_POINT('',(-2.1198426468477,8.,336.998776585022));
#10896=CARTESIAN_POINT('Origin',(-1.88783238349926,8.,315.));
#10897=CARTESIAN_POINT('Origin',(-2.35185291019846,8.,315.));
#10898=CARTESIAN_POINT('',(-5.88783238349923,8.,328.556349186104));
#10899=CARTESIAN_POINT('Origin',(-1.88783238349926,8.,328.556349186104));
#10900=CARTESIAN_POINT('Origin',(-1.88783238349926,6.,328.556349186104));
#10901=CARTESIAN_POINT('',(-5.88783238349923,6.,328.556349186104));
#10902=CARTESIAN_POINT('Origin',(-1.88783238349926,6.,315.));
#10903=CARTESIAN_POINT('',(-2.1198426468477,6.,336.998776585022));
#10904=CARTESIAN_POINT('Origin',(-2.35185291019846,6.,315.));
#10905=CARTESIAN_POINT('',(16.317900533139,6.,326.637882383191));
#10906=CARTESIAN_POINT('Origin',(-2.11984264684888,-6.,322.999388292511));
#10907=CARTESIAN_POINT('',(16.317900533139,-6.,315.999694146255));
#10908=CARTESIAN_POINT('',(-20.0405545273386,-6.,325.214166745933));
#10909=CARTESIAN_POINT('Origin',(-2.11984264684888,-6.,322.999388292511));
#10910=CARTESIAN_POINT('',(-20.0405545273386,-6.,327.428945199355));
#10911=CARTESIAN_POINT('',(-20.0405545273386,-6.,325.214166745933));
#10912=CARTESIAN_POINT('',(-2.1198426468477,-6.,336.998776585022));
#10913=CARTESIAN_POINT('Origin',(-1.88783238349926,-6.,315.));
#10914=CARTESIAN_POINT('',(16.317900533139,-6.,326.637882383191));
#10915=CARTESIAN_POINT('Origin',(-2.35185291019846,-6.,315.));
#10916=CARTESIAN_POINT('',(16.317900533139,-6.,315.999694146255));
#10917=CARTESIAN_POINT('',(-5.88783238349923,-6.,328.556349186104));
#10918=CARTESIAN_POINT('Origin',(-1.88783238349926,-6.,328.556349186104));
#10919=CARTESIAN_POINT('Origin',(16.317900533139,-8.,309.));
#10920=CARTESIAN_POINT('',(16.317900533139,-8.,326.637882383191));
#10921=CARTESIAN_POINT('',(16.317900533139,-8.,326.637882383191));
#10922=CARTESIAN_POINT('',(16.317900533139,-8.,315.999694146255));
#10923=CARTESIAN_POINT('Origin',(-20.0405545273386,-8.,327.428945199355));
#10924=CARTESIAN_POINT('',(-20.0405545273386,-8.,327.428945199355));
#10925=CARTESIAN_POINT('',(-20.0405545273386,-8.,325.214166745933));
#10926=CARTESIAN_POINT('',(-20.0405545273386,-8.,327.428945199355));
#10927=CARTESIAN_POINT('Origin',(-1.88783238349926,-8.,328.556349186104));
#10928=CARTESIAN_POINT('',(-5.88783238349923,-8.,328.556349186104));
#10929=CARTESIAN_POINT('Origin',(-1.88783238349926,-8.,328.556349186104));
#10930=CARTESIAN_POINT('',(-5.88783238349923,-8.,328.556349186104));
#10931=CARTESIAN_POINT('Origin',(-1.88783238349926,-8.,315.));
#10932=CARTESIAN_POINT('',(-2.1198426468477,-8.,336.998776585022));
#10933=CARTESIAN_POINT('Origin',(-1.88783238349926,-8.,315.));
#10934=CARTESIAN_POINT('',(-2.1198426468477,-8.,336.998776585022));
#10935=CARTESIAN_POINT('Origin',(-2.35185291019846,-8.,315.));
#10936=CARTESIAN_POINT('Origin',(-2.35185291019846,-8.,315.));
#10937=CARTESIAN_POINT('Origin',(-2.11984264684888,-8.,322.999388292511));
#10938=CARTESIAN_POINT('',(0.,0.,0.));
#10939=CARTESIAN_POINT('Origin',(-33.7561270252576,0.,302.151410108095));
#10940=CARTESIAN_POINT('',(-32.6699490794746,2.10841540797695,304.52294196412));
#10941=CARTESIAN_POINT('',(-32.6699490795102,2.1084154079953,304.328189117937));
#10942=CARTESIAN_POINT('',(-32.6699490794746,2.10841540797695,302.151410108095));
#10943=CARTESIAN_POINT('',(-35.133102683896,-1.9310971228857,304.000068852074));
#10944=CARTESIAN_POINT('Ctrl Pts',(-35.133102683896,-1.9310971228857,304.000068852074));
#10945=CARTESIAN_POINT('Ctrl Pts',(-35.0694875830777,-1.9764580963502,304.005341754287));
#10946=CARTESIAN_POINT('Ctrl Pts',(-35.003498681129,-2.0187646946572,304.0106146565));
#10947=CARTESIAN_POINT('Ctrl Pts',(-34.9354651692809,-2.05775596331338,
304.015887558713));
#10948=CARTESIAN_POINT('Ctrl Pts',(-34.8647099473273,-2.09830709455844,
304.021371405662));
#10949=CARTESIAN_POINT('Ctrl Pts',(-34.7917434392969,-2.13527166672132,
304.026855252612));
#10950=CARTESIAN_POINT('Ctrl Pts',(-34.7169726735715,-2.16840349165374,
304.032339099561));
#10951=CARTESIAN_POINT('Ctrl Pts',(-34.6452583963628,-2.20018094978974,
304.037598777144));
#10952=CARTESIAN_POINT('Ctrl Pts',(-34.5718849778249,-2.22843266779446,
304.042858454727));
#10953=CARTESIAN_POINT('Ctrl Pts',(-34.4972378823615,-2.25298751882534,
304.048118132309));
#10954=CARTESIAN_POINT('Ctrl Pts',(-34.4226319693529,-2.27752882305931,
304.053374908152));
#10955=CARTESIAN_POINT('Ctrl Pts',(-34.3467542284446,-2.29837715672903,
304.058631683995));
#10956=CARTESIAN_POINT('Ctrl Pts',(-34.2700087638124,-2.31541003307836,
304.063888459838));
#10957=CARTESIAN_POINT('Ctrl Pts',(-34.1932804682484,-2.33243909892737,
304.069144059664));
#10958=CARTESIAN_POINT('Ctrl Pts',(-34.1156853028774,-2.34565429840249,
304.07439965949));
#10959=CARTESIAN_POINT('Ctrl Pts',(-34.0376395453986,-2.35498381385177,
304.079655259316));
#10960=CARTESIAN_POINT('Ctrl Pts',(-33.9595856504682,-2.36431430204428,
304.084911407119));
#10961=CARTESIAN_POINT('Ctrl Pts',(-33.8810815471019,-2.36975824789373,
304.090167554921));
#10962=CARTESIAN_POINT('Ctrl Pts',(-33.8025490068216,-2.37129565051001,
304.095423702723));
#10963=CARTESIAN_POINT('Ctrl Pts',(-33.723934956216,-2.3728346488239,304.100685305974));
#10964=CARTESIAN_POINT('Ctrl Pts',(-33.6452928903964,-2.37045900619068,
304.105946909226));
#10965=CARTESIAN_POINT('Ctrl Pts',(-33.5670440657278,-2.3642008579889,304.111208512478));
#10966=CARTESIAN_POINT('Ctrl Pts',(-33.4887470148127,-2.35793885277075,
304.116473358556));
#10967=CARTESIAN_POINT('Ctrl Pts',(-33.4108441623262,-2.34778964589175,
304.121738204635));
#10968=CARTESIAN_POINT('Ctrl Pts',(-33.3337485462396,-2.33383685868624,
304.127003050713));
#10969=CARTESIAN_POINT('Ctrl Pts',(-33.2565304255633,-2.31986190056416,
304.132276262608));
#10970=CARTESIAN_POINT('Ctrl Pts',(-33.1801225653048,-2.30207141758808,
304.137549474504));
#10971=CARTESIAN_POINT('Ctrl Pts',(-33.1049239604095,-2.28059918241509,
304.142822686399));
#10972=CARTESIAN_POINT('Ctrl Pts',(-33.0826909043258,-2.27425074803247,
304.144381752767));
#10973=CARTESIAN_POINT('Ctrl Pts',(-33.0605634223953,-2.26758079988008,
304.145940819135));
#10974=CARTESIAN_POINT('Ctrl Pts',(-33.0385514704231,-2.26059359142769,
304.147499885503));
#10975=CARTESIAN_POINT('Ctrl Pts',(-32.9631613635555,-2.23666266551085,
304.152839629122));
#10976=CARTESIAN_POINT('Ctrl Pts',(-32.8888314869022,-2.20891240408737,
304.158179372741));
#10977=CARTESIAN_POINT('Ctrl Pts',(-32.8159756387904,-2.17745572469886,
304.163519116361));
#10978=CARTESIAN_POINT('Ctrl Pts',(-32.7432229658767,-2.14604359285473,
304.168851298074));
#10979=CARTESIAN_POINT('Ctrl Pts',(-32.6719406011688,-2.11093565139043,
304.174183479787));
#10980=CARTESIAN_POINT('Ctrl Pts',(-32.6025265181288,-2.07229436433442,
304.1795156615));
#10981=CARTESIAN_POINT('Ctrl Pts',(-32.5331907392874,-2.03369666749643,
304.184841828119));
#10982=CARTESIAN_POINT('Ctrl Pts',(-32.4657194599147,-1.99157377244779,
304.190167994738));
#10983=CARTESIAN_POINT('Ctrl Pts',(-32.4004886439478,-1.94613530917556,
304.195494161357));
#10984=CARTESIAN_POINT('Ctrl Pts',(-32.3352980304424,-1.90072485012248,
304.200817045402));
#10985=CARTESIAN_POINT('Ctrl Pts',(-32.2723455217536,-1.85200314549746,
304.206139929447));
#10986=CARTESIAN_POINT('Ctrl Pts',(-32.2119794855934,-1.80022399668736,
304.211462813492));
#10987=CARTESIAN_POINT('Ctrl Pts',(-32.1516320067756,-1.74846076549336,
304.216784061209));
#10988=CARTESIAN_POINT('Ctrl Pts',(-32.0938697758154,-1.69364226066575,
304.222105308927));
#10989=CARTESIAN_POINT('Ctrl Pts',(-32.0390081820352,-1.63606263350478,
304.227426556645));
#10990=CARTESIAN_POINT('Ctrl Pts',(-31.9841465073673,-1.57848292144862,
304.232747812208));
#10991=CARTESIAN_POINT('Ctrl Pts',(-31.9321857996217,-1.51814241821111,
304.238069067771));
#10992=CARTESIAN_POINT('Ctrl Pts',(-31.8834036289627,-1.45537113598888,
304.243390323335));
#10993=CARTESIAN_POINT('Ctrl Pts',(-31.8345721355805,-1.39253638691941,
304.248716959118));
#10994=CARTESIAN_POINT('Ctrl Pts',(-31.7889258863432,-1.32726631919432,
304.254043594902));
#10995=CARTESIAN_POINT('Ctrl Pts',(-31.7467008958156,-1.25992249476528,
304.259370230685));
#10996=CARTESIAN_POINT('Ctrl Pts',(-31.7044552699207,-1.19254575938631,
304.264699469597));
#10997=CARTESIAN_POINT('Ctrl Pts',(-31.6656344619511,-1.1230936566465,304.270028708509));
#10998=CARTESIAN_POINT('Ctrl Pts',(-31.6304287304042,-1.0519528609959,304.275357947421));
#10999=CARTESIAN_POINT('Ctrl Pts',(-31.5951589238931,-0.980682588020334,
304.280696885629));
#11000=CARTESIAN_POINT('Ctrl Pts',(-31.5635175276295,-0.907717910366174,
304.286035823837));
#11001=CARTESIAN_POINT('Ctrl Pts',(-31.5356467269886,-0.833465840631194,
304.291374762044));
#11002=CARTESIAN_POINT('Ctrl Pts',(-31.5094819150593,-0.763758785387225,
304.296386900587));
#11003=CARTESIAN_POINT('Ctrl Pts',(-31.4866398483132,-0.692917589734796,
304.301399039129));
#11004=CARTESIAN_POINT('Ctrl Pts',(-31.4671973727891,-0.62128826526054,
304.306411177672));
#11005=CARTESIAN_POINT('Ctrl Pts',(-31.4465296698883,-0.545144998659011,
304.311739171536));
#11006=CARTESIAN_POINT('Ctrl Pts',(-31.4296258778281,-0.467823027100496,
304.3170671654));
#11007=CARTESIAN_POINT('Ctrl Pts',(-31.4166165369438,-0.389729056614872,
304.322395159264));
#11008=CARTESIAN_POINT('Ctrl Pts',(-31.4036261558074,-0.311748899887667,
304.327715388137));
#11009=CARTESIAN_POINT('Ctrl Pts',(-31.3945190316741,-0.232999437688756,
304.33303561701));
#11010=CARTESIAN_POINT('Ctrl Pts',(-31.3893755614233,-0.153901172634812,
304.338355845883));
#11011=CARTESIAN_POINT('Ctrl Pts',(-31.3842381475483,-0.0748960448578465,
304.343669810248));
#11012=CARTESIAN_POINT('Ctrl Pts',(-31.383055143537,0.00445660346383708,
304.348983774614));
#11013=CARTESIAN_POINT('Ctrl Pts',(-31.3858554128096,0.0837290016837932,
304.35429773898));
#11014=CARTESIAN_POINT('Ctrl Pts',(-31.3886538752934,0.162950251796037,
304.359608274672));
#11015=CARTESIAN_POINT('Ctrl Pts',(-31.3954304936321,0.242090886526085,
304.364918810363));
#11016=CARTESIAN_POINT('Ctrl Pts',(-31.4061620604436,0.320722195438071,
304.370229346055));
#11017=CARTESIAN_POINT('Ctrl Pts',(-31.4168900604234,0.399327369802875,
304.375538116693));
#11018=CARTESIAN_POINT('Ctrl Pts',(-31.4315703353571,0.477423089519046,
304.380846887332));
#11019=CARTESIAN_POINT('Ctrl Pts',(-31.4501278790099,0.554586332327998,
304.38615565797));
#11020=CARTESIAN_POINT('Ctrl Pts',(-31.4686850603757,0.631748068728147,
304.391464324969));
#11021=CARTESIAN_POINT('Ctrl Pts',(-31.4911192489282,0.70797690809233,304.396772991968));
#11022=CARTESIAN_POINT('Ctrl Pts',(-31.5173047749994,0.782862053141504,
304.402081658966));
#11023=CARTESIAN_POINT('Ctrl Pts',(-31.543516409334,0.857821862380335,304.407395618968));
#11024=CARTESIAN_POINT('Ctrl Pts',(-31.5734866975547,0.931434856612447,
304.41270957897));
#11025=CARTESIAN_POINT('Ctrl Pts',(-31.6070409009699,1.0033079750975,304.418023538972));
#11026=CARTESIAN_POINT('Ctrl Pts',(-31.6406111111443,1.0752153800676,304.423340033956));
#11027=CARTESIAN_POINT('Ctrl Pts',(-31.677768422223,1.14538084027812,304.428656528939));
#11028=CARTESIAN_POINT('Ctrl Pts',(-31.7182921612011,1.21343608374556,304.433973023922));
#11029=CARTESIAN_POINT('Ctrl Pts',(-31.7588901001272,1.28161593801295,304.439299253537));
#11030=CARTESIAN_POINT('Ctrl Pts',(-31.8028665231676,1.34767746266607,304.444625483151));
#11031=CARTESIAN_POINT('Ctrl Pts',(-31.8499575801153,1.41128172556225,304.449951712766));
#11032=CARTESIAN_POINT('Ctrl Pts',(-31.8952569913421,1.47246607451222,304.455075298457));
#11033=CARTESIAN_POINT('Ctrl Pts',(-31.9434380280056,1.53137651453439,304.460198884149));
#11034=CARTESIAN_POINT('Ctrl Pts',(-31.9942333057017,1.58774323600805,304.465322469841));
#11035=CARTESIAN_POINT('Ctrl Pts',(-32.0470827982975,1.64638948747656,304.470653258772));
#11036=CARTESIAN_POINT('Ctrl Pts',(-32.1029637711113,1.70250526679375,304.475984047703));
#11037=CARTESIAN_POINT('Ctrl Pts',(-32.1616044026078,1.75576070931038,304.481314836634));
#11038=CARTESIAN_POINT('Ctrl Pts',(-32.2201707660216,1.8089487040607,304.486638874146));
#11039=CARTESIAN_POINT('Ctrl Pts',(-32.2814895103399,1.85928323676079,304.491962911658));
#11040=CARTESIAN_POINT('Ctrl Pts',(-32.3452499759995,1.90646899119202,304.49728694917));
#11041=CARTESIAN_POINT('Ctrl Pts',(-32.408939174419,1.95360200450137,304.502605035824));
#11042=CARTESIAN_POINT('Ctrl Pts',(-32.4750642973849,1.9975929542515,304.507923122478));
#11043=CARTESIAN_POINT('Ctrl Pts',(-32.5432806701215,2.03818590450751,304.513241209133));
#11044=CARTESIAN_POINT('Ctrl Pts',(-32.5847586402436,2.06286785563367,304.516474794129));
#11045=CARTESIAN_POINT('Ctrl Pts',(-32.6270090988392,2.08629431182957,304.519708379124));
#11046=CARTESIAN_POINT('Ctrl Pts',(-32.6699490794746,2.10841540797695,304.52294196412));
#11047=CARTESIAN_POINT('',(-32.3791022351265,-1.93106208855757,304.));
#11048=CARTESIAN_POINT('Origin',(-33.7561270252576,0.,304.));
#11049=CARTESIAN_POINT('Ctrl Pts',(-32.3791022351265,-1.93106208855758,
304.));
#11050=CARTESIAN_POINT('Ctrl Pts',(-32.372383794194,-1.92627122255186,304.000553722788));
#11051=CARTESIAN_POINT('Ctrl Pts',(-32.365690294893,-1.92144525176054,304.001105480632));
#11052=CARTESIAN_POINT('Ctrl Pts',(-32.351055489904,-1.91077712792039,304.002312345817));
#11053=CARTESIAN_POINT('Ctrl Pts',(-32.3431251147181,-1.90492017144399,
304.002966647622));
#11054=CARTESIAN_POINT('Ctrl Pts',(-32.3123044268341,-1.88185926415591,
304.005511672187));
#11055=CARTESIAN_POINT('Ctrl Pts',(-32.2896890562164,-1.86429016234149,
304.007383786941));
#11056=CARTESIAN_POINT('Ctrl Pts',(-32.1433176031211,-1.74626715523718,
304.019567842445));
#11057=CARTESIAN_POINT('Ctrl Pts',(-32.029629893516,-1.6339581815929,304.02937038556));
#11058=CARTESIAN_POINT('Ctrl Pts',(-31.8625511884864,-1.43183153393863,
304.045807677244));
#11059=CARTESIAN_POINT('Ctrl Pts',(-31.8022683225534,-1.34840805993611,
304.052310383391));
#11060=CARTESIAN_POINT('Ctrl Pts',(-31.7294611830989,-1.23247143628013,
304.061207693097));
#11061=CARTESIAN_POINT('Ctrl Pts',(-31.7119560853931,-1.2032145583658,304.063441326482));
#11062=CARTESIAN_POINT('Ctrl Pts',(-31.6828615830205,-1.15211935922127,
304.067329597822));
#11063=CARTESIAN_POINT('Ctrl Pts',(-31.6709715775492,-1.13045800411972,
304.068974179702));
#11064=CARTESIAN_POINT('Ctrl Pts',(-31.6470762526234,-1.08526520511566,
304.07240012123));
#11065=CARTESIAN_POINT('Ctrl Pts',(-31.6351213442428,-1.06171113614403,
304.074182843954));
#11066=CARTESIAN_POINT('Ctrl Pts',(-31.6046373686383,-0.999079775851659,
304.078918926595));
#11067=CARTESIAN_POINT('Ctrl Pts',(-31.5867801472149,-0.959688416450391,
304.081893480809));
#11068=CARTESIAN_POINT('Ctrl Pts',(-31.5011751545305,-0.756235746958286,
304.097252202384));
#11069=CARTESIAN_POINT('Ctrl Pts',(-31.4509327899566,-0.585455956005303,
304.110186955138));
#11070=CARTESIAN_POINT('Ctrl Pts',(-31.4040698176274,-0.318920429501764,
304.130075262116));
#11071=CARTESIAN_POINT('Ctrl Pts',(-31.3933547949862,-0.2262574943469,304.136923917303));
#11072=CARTESIAN_POINT('Ctrl Pts',(-31.3852061838439,-0.0813934329749035,
304.147360545508));
#11073=CARTESIAN_POINT('Ctrl Pts',(-31.3839927149568,-0.0295001198401178,
304.151044748579));
#11074=CARTESIAN_POINT('Ctrl Pts',(-31.3846576241952,0.0409130542434561,
304.155937841315));
#11075=CARTESIAN_POINT('Ctrl Pts',(-31.3850493654905,0.0594288202409265,
304.157214556448));
#11076=CARTESIAN_POINT('Ctrl Pts',(-31.3860773174482,0.0906934458287153,
304.159351557626));
#11077=CARTESIAN_POINT('Ctrl Pts',(-31.3865996294996,0.103445005545772,
304.160217859862));
#11078=CARTESIAN_POINT('Ctrl Pts',(-31.3879186001374,0.130335865156393,
304.162032829539));
#11079=CARTESIAN_POINT('Ctrl Pts',(-31.3887389998056,0.144473339197381,
304.162980170615));
#11080=CARTESIAN_POINT('Ctrl Pts',(-31.3914324490789,0.184661013930785,
304.165655857413));
#11081=CARTESIAN_POINT('Ctrl Pts',(-31.3936092732913,0.210689678850066,
304.167368196035));
#11082=CARTESIAN_POINT('Ctrl Pts',(-31.408759857812,0.36175558652666,304.177214760618));
#11083=CARTESIAN_POINT('Ctrl Pts',(-31.4312295616042,0.485653295681868,
304.184932480841));
#11084=CARTESIAN_POINT('Ctrl Pts',(-31.4907951271127,0.710565841075942,
304.199207257352));
#11085=CARTESIAN_POINT('Ctrl Pts',(-31.5251293607131,0.811960750388482,
304.205748774764));
#11086=CARTESIAN_POINT('Ctrl Pts',(-31.5918300990257,0.972356665312212,
304.216653188886));
#11087=CARTESIAN_POINT('Ctrl Pts',(-31.6200661485106,1.03290917980854,304.220905457598));
#11088=CARTESIAN_POINT('Ctrl Pts',(-31.6638603280129,1.11732731735751,304.227085539766));
#11089=CARTESIAN_POINT('Ctrl Pts',(-31.6773519155927,1.14223211051689,304.228941083339));
#11090=CARTESIAN_POINT('Ctrl Pts',(-31.7018742494461,1.18562505501877,304.232235225492));
#11091=CARTESIAN_POINT('Ctrl Pts',(-31.7127169367836,1.2042160913737,304.233666799671));
#11092=CARTESIAN_POINT('Ctrl Pts',(-31.7360493754349,1.24299958800252,304.23669771837));
#11093=CARTESIAN_POINT('Ctrl Pts',(-31.7485922774706,1.26315709619378,304.238298959829));
#11094=CARTESIAN_POINT('Ctrl Pts',(-31.7832034831385,1.31696232430415,304.242645578171));
#11095=CARTESIAN_POINT('Ctrl Pts',(-31.8058280346489,1.3502409247028,304.245412136589));
#11096=CARTESIAN_POINT('Ctrl Pts',(-31.9430749518018,1.54146795382015,304.261785416916));
#11097=CARTESIAN_POINT('Ctrl Pts',(-32.0759767677403,1.68533294663214,304.276143635163));
#11098=CARTESIAN_POINT('Ctrl Pts',(-32.2812087133711,1.85882772557642,304.295885295031));
#11099=CARTESIAN_POINT('Ctrl Pts',(-32.3396540123282,1.90374107562473,304.30127104078));
#11100=CARTESIAN_POINT('Ctrl Pts',(-32.4363786513325,1.9711463092728,304.309717051742));
#11101=CARTESIAN_POINT('Ctrl Pts',(-32.4733619057364,1.99541169177774,304.312844363311));
#11102=CARTESIAN_POINT('Ctrl Pts',(-32.5253632199481,2.02748689632691,304.317080377009));
#11103=CARTESIAN_POINT('Ctrl Pts',(-32.539816164388,2.03619021541879,304.318241011223));
#11104=CARTESIAN_POINT('Ctrl Pts',(-32.5649011618963,2.05093355995385,304.320225156927));
#11105=CARTESIAN_POINT('Ctrl Pts',(-32.5754883891497,2.05704641372135,304.321053285514));
#11106=CARTESIAN_POINT('Ctrl Pts',(-32.5987250625579,2.07022429727514,304.322851050667));
#11107=CARTESIAN_POINT('Ctrl Pts',(-32.6113925350712,2.07725562192876,304.323818552738));
#11108=CARTESIAN_POINT('Ctrl Pts',(-32.6393100146382,2.09241880908629,304.325925222684));
#11109=CARTESIAN_POINT('Ctrl Pts',(-32.6545859334898,2.10050088113243,304.327061439715));
#11110=CARTESIAN_POINT('Ctrl Pts',(-32.6699490795102,2.1084154079953,304.328189117937));
#11111=CARTESIAN_POINT('Origin',(-33.7561270252576,0.,302.151410108095));
#11112=CARTESIAN_POINT('',(-32.6699490731211,2.10841540470388,305.524079281032));
#11113=CARTESIAN_POINT('',(-32.6699493942465,2.1084155701358,305.324530114841));
#11114=CARTESIAN_POINT('',(-32.6699490794746,2.10841540797695,302.151410108095));
#11115=CARTESIAN_POINT('',(-36.1278767663821,0.00110814072209554,304.848589891855));
#11116=CARTESIAN_POINT('Ctrl Pts',(-32.6699490731214,2.10841540470401,305.524079281032));
#11117=CARTESIAN_POINT('Ctrl Pts',(-32.6181216565324,2.08171582876206,305.520434275554));
#11118=CARTESIAN_POINT('Ctrl Pts',(-32.5672521921668,2.05309167355925,305.516743827637));
#11119=CARTESIAN_POINT('Ctrl Pts',(-32.4854943209372,2.00302137170522,305.510578700104));
#11120=CARTESIAN_POINT('Ctrl Pts',(-32.454010028249,1.98269845406367,305.508144832193));
#11121=CARTESIAN_POINT('Ctrl Pts',(-32.4034285920564,1.94832394525082,305.504127258202));
#11122=CARTESIAN_POINT('Ctrl Pts',(-32.3840367160886,1.93471635174277,305.502560304462));
#11123=CARTESIAN_POINT('Ctrl Pts',(-32.3465602066406,1.90757164974185,305.499477388479));
#11124=CARTESIAN_POINT('Ctrl Pts',(-32.3284586877127,1.8940621087477,305.497962606613));
#11125=CARTESIAN_POINT('Ctrl Pts',(-32.2855166339777,1.86104821955232,305.494305251938));
#11126=CARTESIAN_POINT('Ctrl Pts',(-32.2608679295274,1.84130265490888,305.492153274022));
#11127=CARTESIAN_POINT('Ctrl Pts',(-32.1688030044336,1.76448352823755,305.48390821089));
#11128=CARTESIAN_POINT('Ctrl Pts',(-32.1042062859053,1.70415792351539,305.477685449562));
#11129=CARTESIAN_POINT('Ctrl Pts',(-31.9102167026194,1.50158038130959,305.457568101374));
#11130=CARTESIAN_POINT('Ctrl Pts',(-31.7946758074913,1.34715674638086,305.443270458497));
#11131=CARTESIAN_POINT('Ctrl Pts',(-31.6798467494391,1.14705896648543,305.426868389652));
#11132=CARTESIAN_POINT('Ctrl Pts',(-31.6614765686871,1.1131594325377,305.424158539114));
#11133=CARTESIAN_POINT('Ctrl Pts',(-31.6370000137217,1.06523778711765,305.420437545151));
#11134=CARTESIAN_POINT('Ctrl Pts',(-31.6301912445061,1.05158353027739,305.41938949495));
#11135=CARTESIAN_POINT('Ctrl Pts',(-31.617966898918,1.02646483382323,305.417484921128));
#11136=CARTESIAN_POINT('Ctrl Pts',(-31.6125106258224,1.01502095753611,305.416626059093));
#11137=CARTESIAN_POINT('Ctrl Pts',(-31.6009915845908,0.99035390809909,305.414794249643));
#11138=CARTESIAN_POINT('Ctrl Pts',(-31.5949583155752,0.977117939095003,
305.413823026405));
#11139=CARTESIAN_POINT('Ctrl Pts',(-31.5778821625025,0.93872370948763,305.41103701726));
#11140=CARTESIAN_POINT('Ctrl Pts',(-31.5671537626555,0.91342711756605,305.409239861761));
#11141=CARTESIAN_POINT('Ctrl Pts',(-31.5171338724186,0.789538453185028,
305.400596970975));
#11142=CARTESIAN_POINT('Ctrl Pts',(-31.4840466025184,0.688561335344408,
305.394032332415));
#11143=CARTESIAN_POINT('Ctrl Pts',(-31.4137832117428,0.41284580156758,305.376556719394));
#11144=CARTESIAN_POINT('Ctrl Pts',(-31.3893771465728,0.235594430216639,
305.365743369847));
#11145=CARTESIAN_POINT('Ctrl Pts',(-31.3841509149287,0.0192899891988883,
305.351837760297));
#11146=CARTESIAN_POINT('Ctrl Pts',(-31.3841464266578,-0.0187229822491736,
305.349370046344));
#11147=CARTESIAN_POINT('Ctrl Pts',(-31.3856243381822,-0.0805064373339045,
305.345311372373));
#11148=CARTESIAN_POINT('Ctrl Pts',(-31.3865513222008,-0.104284197700153,
305.343737860391));
#11149=CARTESIAN_POINT('Ctrl Pts',(-31.3890521442885,-0.150539455882248,
305.340652496818));
#11150=CARTESIAN_POINT('Ctrl Pts',(-31.3905888490534,-0.173016461854979,
305.339141977042));
#11151=CARTESIAN_POINT('Ctrl Pts',(-31.3950198481144,-0.226598106673857,
305.33551274049));
#11152=CARTESIAN_POINT('Ctrl Pts',(-31.3982088666395,-0.257673433709,305.333384988067));
#11153=CARTESIAN_POINT('Ctrl Pts',(-31.4123690306273,-0.373148004602919,
305.325388757618));
#11154=CARTESIAN_POINT('Ctrl Pts',(-31.4272654415711,-0.456992025248043,
305.319400793902));
#11155=CARTESIAN_POINT('Ctrl Pts',(-31.4858069850722,-0.70743619402694,
305.300981347359));
#11156=CARTESIAN_POINT('Ctrl Pts',(-31.5431018911505,-0.870248190707576,
305.288238017824));
#11157=CARTESIAN_POINT('Ctrl Pts',(-31.642056148665,-1.07662778785411,305.27176955701));
#11158=CARTESIAN_POINT('Ctrl Pts',(-31.6684422114981,-1.1269411178138,305.267732675978));
#11159=CARTESIAN_POINT('Ctrl Pts',(-31.7062482664399,-1.19313566260966,
305.262435535179));
#11160=CARTESIAN_POINT('Ctrl Pts',(-31.7160925243171,-1.20989046296971,
305.261096035152));
#11161=CARTESIAN_POINT('Ctrl Pts',(-31.7327447513185,-1.23745111211543,
305.258897141823));
#11162=CARTESIAN_POINT('Ctrl Pts',(-31.7394359244163,-1.24832612573336,
305.25803069155));
#11163=CARTESIAN_POINT('Ctrl Pts',(-31.7536136304817,-1.27095727132005,
305.256230867488));
#11164=CARTESIAN_POINT('Ctrl Pts',(-31.7611164867596,-1.28270232624646,
305.255298556012));
#11165=CARTESIAN_POINT('Ctrl Pts',(-31.7820880874436,-1.31490231416333,
305.252745417354));
#11166=CARTESIAN_POINT('Ctrl Pts',(-31.7957711945606,-1.3352164455795,305.251137935039));
#11167=CARTESIAN_POINT('Ctrl Pts',(-31.8277389507178,-1.38112511928629,
305.247503579465));
#11168=CARTESIAN_POINT('Ctrl Pts',(-31.846223205704,-1.4065755412505,305.245487661209));
#11169=CARTESIAN_POINT('Ctrl Pts',(-31.9114730003668,-1.4927571065043,305.238629039777));
#11170=CARTESIAN_POINT('Ctrl Pts',(-31.9606747638233,-1.55158787637714,
305.23388967039));
#11171=CARTESIAN_POINT('Ctrl Pts',(-32.1364737003043,-1.74220667171159,
305.217954213384));
#11172=CARTESIAN_POINT('Ctrl Pts',(-32.2753877912973,-1.86171046637986,
305.206896218619));
#11173=CARTESIAN_POINT('Ctrl Pts',(-32.4576412969985,-1.98507806684135,
305.192743224935));
#11174=CARTESIAN_POINT('Ctrl Pts',(-32.4891405869647,-2.00532920800316,
305.190311002364));
#11175=CARTESIAN_POINT('Ctrl Pts',(-32.5413247513177,-2.03715842597403,
305.186295403946));
#11176=CARTESIAN_POINT('Ctrl Pts',(-32.5617277762762,-2.04918749331368,
305.184728746464));
#11177=CARTESIAN_POINT('Ctrl Pts',(-32.6019362513427,-2.07208880768021,
305.181645882816));
#11178=CARTESIAN_POINT('Ctrl Pts',(-32.6217237007363,-2.08298761531809,
305.180130849391));
#11179=CARTESIAN_POINT('Ctrl Pts',(-32.6695564107046,-2.10844987059365,
305.176471969222));
#11180=CARTESIAN_POINT('Ctrl Pts',(-32.697742294909,-2.12273836150287,305.174318698113));
#11181=CARTESIAN_POINT('Ctrl Pts',(-32.805925583813,-2.17489028993111,305.166060163608));
#11182=CARTESIAN_POINT('Ctrl Pts',(-32.8877261450782,-2.20882483112531,
305.159824665474));
#11183=CARTESIAN_POINT('Ctrl Pts',(-33.1537677640361,-2.30212562174332,
305.139602004255));
#11184=CARTESIAN_POINT('Ctrl Pts',(-33.3434431248135,-2.3435666723399,305.125205540751));
#11185=CARTESIAN_POINT('Ctrl Pts',(-33.5730667055112,-2.3649672452909,305.108824015106));
#11186=CARTESIAN_POINT('Ctrl Pts',(-33.6101746946479,-2.36754713408198,
305.10621142543));
#11187=CARTESIAN_POINT('Ctrl Pts',(-33.6625234416,-2.36995100138893,305.102588141953));
#11188=CARTESIAN_POINT('Ctrl Pts',(-33.6777234198243,-2.37050253852458,
305.101543482546));
#11189=CARTESIAN_POINT('Ctrl Pts',(-33.7055934205733,-2.37124544078164,
305.099642857348));
#11190=CARTESIAN_POINT('Ctrl Pts',(-33.7182615593693,-2.37148156710566,
305.098784597087));
#11191=CARTESIAN_POINT('Ctrl Pts',(-33.7455149831232,-2.37177109754041,
305.096950865752));
#11192=CARTESIAN_POINT('Ctrl Pts',(-33.760099723317,-2.37179151700474,305.095977163844));
#11193=CARTESIAN_POINT('Ctrl Pts',(-33.8023392391489,-2.37146101419212,
305.093176851555));
#11194=CARTESIAN_POINT('Ctrl Pts',(-33.8299898477957,-2.37076092330193,
305.091368141484));
#11195=CARTESIAN_POINT('Ctrl Pts',(-33.8946318827031,-2.36799210594985,
305.087183606622));
#11196=CARTESIAN_POINT('Ctrl Pts',(-33.931600224627,-2.36554003461956,305.084824153858));
#11197=CARTESIAN_POINT('Ctrl Pts',(-34.0711930949718,-2.35299022398947,
305.075991871651));
#11198=CARTESIAN_POINT('Ctrl Pts',(-34.1731832714032,-2.3370700185528,305.069693111292));
#11199=CARTESIAN_POINT('Ctrl Pts',(-34.4099525970118,-2.28411246821819,
305.05482454512));
#11200=CARTESIAN_POINT('Ctrl Pts',(-34.5431206747547,-2.2417165620999,305.046254938475));
#11201=CARTESIAN_POINT('Ctrl Pts',(-34.7089579750039,-2.17231100895509,
305.034728193582));
#11202=CARTESIAN_POINT('Ctrl Pts',(-34.7457266360603,-2.15580941662165,
305.032116895528));
#11203=CARTESIAN_POINT('Ctrl Pts',(-34.8039228525743,-2.12788867601317,
305.027883030112));
#11204=CARTESIAN_POINT('Ctrl Pts',(-34.8256273284665,-2.1170629044455,305.026280962068));
#11205=CARTESIAN_POINT('Ctrl Pts',(-34.8670028425869,-2.09562695551453,
305.023180228047));
#11206=CARTESIAN_POINT('Ctrl Pts',(-34.8866974921257,-2.08506781148047,
305.021683494114));
#11207=CARTESIAN_POINT('Ctrl Pts',(-34.9324881557618,-2.05967797867248,
305.018152936988));
#11208=CARTESIAN_POINT('Ctrl Pts',(-34.9584571323438,-2.04462736319817,
305.016111381013));
#11209=CARTESIAN_POINT('Ctrl Pts',(-35.048137862753,-1.99035253807139,305.008918871316));
#11210=CARTESIAN_POINT('Ctrl Pts',(-35.1102679548164,-1.94861373796396,
305.003678229668));
#11211=CARTESIAN_POINT('Ctrl Pts',(-35.273642641933,-1.82726854838893,304.989180911537));
#11212=CARTESIAN_POINT('Ctrl Pts',(-35.3705423976899,-1.74224616564757,
304.979764130925));
#11213=CARTESIAN_POINT('Ctrl Pts',(-35.5293607819236,-1.578216152808,304.9631006366));
#11214=CARTESIAN_POINT('Ctrl Pts',(-35.5940909633752,-1.50233693668429,
304.955864831576));
#11215=CARTESIAN_POINT('Ctrl Pts',(-35.6697542502341,-1.40140323059667,
304.947005728748));
#11216=CARTESIAN_POINT('Ctrl Pts',(-35.6852920996744,-1.37993566236092,
304.945162494972));
#11217=CARTESIAN_POINT('Ctrl Pts',(-35.7087735485585,-1.34632090606661,
304.942344465875));
#11218=CARTESIAN_POINT('Ctrl Pts',(-35.7169704430909,-1.33435435531888,
304.941354319121));
#11219=CARTESIAN_POINT('Ctrl Pts',(-35.732129446701,-1.3117825270777,304.939512094049));
#11220=CARTESIAN_POINT('Ctrl Pts',(-35.7391166861297,-1.30119598071789,
304.938658508707));
#11221=CARTESIAN_POINT('Ctrl Pts',(-35.7559077787892,-1.2753059491114,304.936595346927));
#11222=CARTESIAN_POINT('Ctrl Pts',(-35.7656212467673,-1.25994497923001,
304.935391565351));
#11223=CARTESIAN_POINT('Ctrl Pts',(-35.8015282977124,-1.20168946429857,
304.930896210252));
#11224=CARTESIAN_POINT('Ctrl Pts',(-35.8265346278844,-1.15807473979308,
304.927671513271));
#11225=CARTESIAN_POINT('Ctrl Pts',(-35.8926687857399,-1.03372682251686,
304.918771002815));
#11226=CARTESIAN_POINT('Ctrl Pts',(-35.9305866432221,-0.951382823163796,
304.913209131072));
#11227=CARTESIAN_POINT('Ctrl Pts',(-35.9833939359804,-0.816934037775414,
304.904355158999));
#11228=CARTESIAN_POINT('Ctrl Pts',(-36.0013710684059,-0.766145041210571,
304.901060175691));
#11229=CARTESIAN_POINT('Ctrl Pts',(-36.0524976455148,-0.604388754233415,
304.890619029732));
#11230=CARTESIAN_POINT('Ctrl Pts',(-36.0792572764916,-0.491594399928589,
304.883406527555));
#11231=CARTESIAN_POINT('Ctrl Pts',(-36.1030786734283,-0.34375945544675,
304.87373898335));
#11232=CARTESIAN_POINT('Ctrl Pts',(-36.1077623370245,-0.310102840630191,
304.871524785634));
#11233=CARTESIAN_POINT('Ctrl Pts',(-36.1141341230659,-0.255791724389269,
304.867924540332));
#11234=CARTESIAN_POINT('Ctrl Pts',(-36.1162775011514,-0.235194737764522,
304.866552931835));
#11235=CARTESIAN_POINT('Ctrl Pts',(-36.1200461649209,-0.193709186586245,
304.863776436969));
#11236=CARTESIAN_POINT('Ctrl Pts',(-36.1216649101111,-0.172821914907311,
304.862371474394));
#11237=CARTESIAN_POINT('Ctrl Pts',(-36.1245600991057,-0.127714479985215,
304.859321057913));
#11238=CARTESIAN_POINT('Ctrl Pts',(-36.1257421368948,-0.103490869569307,
304.857672795567));
#11239=CARTESIAN_POINT('Ctrl Pts',(-36.1274492786462,-0.052431689755752,
304.854176069068));
#11240=CARTESIAN_POINT('Ctrl Pts',(-36.1278907109207,-0.0255970923137018,
304.852325268517));
#11241=CARTESIAN_POINT('Ctrl Pts',(-36.1278767020865,0.00123812836145487,
304.850461017329));
#11242=CARTESIAN_POINT('Ctrl Pts',(-32.6699490794746,2.10841540797695,304.52294196412));
#11243=CARTESIAN_POINT('Ctrl Pts',(-32.7405091890633,2.14476537705674,304.528255476336));
#11244=CARTESIAN_POINT('Ctrl Pts',(-32.812932257405,2.17758811148641,304.533568988553));
#11245=CARTESIAN_POINT('Ctrl Pts',(-32.8868298076994,2.2066989849197,304.538882500769));
#11246=CARTESIAN_POINT('Ctrl Pts',(-32.9607171270794,2.23580582803188,304.544195277344));
#11247=CARTESIAN_POINT('Ctrl Pts',(-33.0360780865893,2.26120165971117,304.549508053919));
#11248=CARTESIAN_POINT('Ctrl Pts',(-33.1125046495563,2.28275016153689,304.554820830494));
#11249=CARTESIAN_POINT('Ctrl Pts',(-33.188944438043,2.30430239230347,304.560134526438));
#11250=CARTESIAN_POINT('Ctrl Pts',(-33.2664497444773,2.32200584587864,304.565448222382));
#11251=CARTESIAN_POINT('Ctrl Pts',(-33.3445992591608,2.33577459533907,304.570761918326));
#11252=CARTESIAN_POINT('Ctrl Pts',(-33.4228355339393,2.34955863060153,304.576081513434));
#11253=CARTESIAN_POINT('Ctrl Pts',(-33.501716981682,2.35939916406787,304.581401108542));
#11254=CARTESIAN_POINT('Ctrl Pts',(-33.5808147186556,2.36526185815733,304.58672070365));
#11255=CARTESIAN_POINT('Ctrl Pts',(-33.6599636679274,2.3711283480828,304.592043742961));
#11256=CARTESIAN_POINT('Ctrl Pts',(-33.7393287168723,2.37301186233046,304.597366782272));
#11257=CARTESIAN_POINT('Ctrl Pts',(-33.8184810139544,2.37093020618356,304.602689821583));
#11258=CARTESIAN_POINT('Ctrl Pts',(-33.8977626590998,2.3688451482631,304.608021559628));
#11259=CARTESIAN_POINT('Ctrl Pts',(-33.9768303922003,2.36278202619957,304.613353297674));
#11260=CARTESIAN_POINT('Ctrl Pts',(-34.055261151041,2.35281041252622,304.61868503572));
#11261=CARTESIAN_POINT('Ctrl Pts',(-34.082468715122,2.34935126815456,304.62053461115));
#11262=CARTESIAN_POINT('Ctrl Pts',(-34.1095997281322,2.34542222903315,304.62238418658));
#11263=CARTESIAN_POINT('Ctrl Pts',(-34.1366369059784,2.34102761478241,304.624233762011));
#11264=CARTESIAN_POINT('Ctrl Pts',(-34.2145896209335,2.32835720539376,304.629566397951));
#11265=CARTESIAN_POINT('Ctrl Pts',(-34.292056016926,2.3117650491669,304.634899033892));
#11266=CARTESIAN_POINT('Ctrl Pts',(-34.3686111942889,2.29130120350557,304.640231669832));
#11267=CARTESIAN_POINT('Ctrl Pts',(-34.4450558691736,2.2708668960902,304.645556608456));
#11268=CARTESIAN_POINT('Ctrl Pts',(-34.5205914884406,2.24657211742218,304.650881547079));
#11269=CARTESIAN_POINT('Ctrl Pts',(-34.5948014173447,2.21851827275714,304.656206485702));
#11270=CARTESIAN_POINT('Ctrl Pts',(-34.6689251554939,2.19049701109124,304.661525239702));
#11271=CARTESIAN_POINT('Ctrl Pts',(-34.7417258269051,2.15872552444736,304.666843993702));
#11272=CARTESIAN_POINT('Ctrl Pts',(-34.8128015615324,2.12335512500579,304.672162747702));
#11273=CARTESIAN_POINT('Ctrl Pts',(-34.8838320994485,2.08800721742789,304.677478119532));
#11274=CARTESIAN_POINT('Ctrl Pts',(-34.9531394592419,2.04906514768656,304.682793491362));
#11275=CARTESIAN_POINT('Ctrl Pts',(-35.0203425103695,2.00672800092669,304.688108863192));
#11276=CARTESIAN_POINT('Ctrl Pts',(-35.0875237492067,1.96440459565812,304.693422509796));
#11277=CARTESIAN_POINT('Ctrl Pts',(-35.1526016393793,1.91868855117903,304.698736156401));
#11278=CARTESIAN_POINT('Ctrl Pts',(-35.2152216968624,1.86982373548807,304.704049803005));
#11279=CARTESIAN_POINT('Ctrl Pts',(-35.2778409241516,1.82095956762904,304.709363379163));
#11280=CARTESIAN_POINT('Ctrl Pts',(-35.3380020148532,1.76894700092991,304.714676955321));
#11281=CARTESIAN_POINT('Ctrl Pts',(-35.3953825992675,1.7140709511503,304.719990531479));
#11282=CARTESIAN_POINT('Ctrl Pts',(-35.4528205361549,1.65914005220532,304.72530941861));
#11283=CARTESIAN_POINT('Ctrl Pts',(-35.5074720755336,1.60134027751406,304.730628305741));
#11284=CARTESIAN_POINT('Ctrl Pts',(-35.5590513093841,1.54099386377976,304.735947192872));
#11285=CARTESIAN_POINT('Ctrl Pts',(-35.6106552997318,1.48061848556279,304.74126863291));
#11286=CARTESIAN_POINT('Ctrl Pts',(-35.6591837602601,1.41769440490141,304.746590072949));
#11287=CARTESIAN_POINT('Ctrl Pts',(-35.7043923572474,1.35257541699771,304.751911512987));
#11288=CARTESIAN_POINT('Ctrl Pts',(-35.7496834151574,1.28733765142383,304.757242659384));
#11289=CARTESIAN_POINT('Ctrl Pts',(-35.7916422609772,1.21989737755875,304.762573805781));
#11290=CARTESIAN_POINT('Ctrl Pts',(-35.8300691345773,1.15063555902402,304.767904952178));
#11291=CARTESIAN_POINT('Ctrl Pts',(-35.8666859914183,1.08463617223471,304.772984986179));
#11292=CARTESIAN_POINT('Ctrl Pts',(-35.9000959840596,1.01698330734997,304.778065020179));
#11293=CARTESIAN_POINT('Ctrl Pts',(-35.930167366497,0.948022498237167,304.78314505418));
#11294=CARTESIAN_POINT('Ctrl Pts',(-35.9649442239047,0.868270919464904,
304.78901999586));
#11295=CARTESIAN_POINT('Ctrl Pts',(-35.9953692123839,0.7865113186969,304.79489493754));
#11296=CARTESIAN_POINT('Ctrl Pts',(-36.0212299042613,0.703211923981057,
304.800769879221));
#11297=CARTESIAN_POINT('Ctrl Pts',(-36.0470153730772,0.620154828872908,
304.806627731988));
#11298=CARTESIAN_POINT('Ctrl Pts',(-36.0682628988544,0.535567149082814,
304.812485584756));
#11299=CARTESIAN_POINT('Ctrl Pts',(-36.0848080894652,0.44993617736413,304.818343437524));
#11300=CARTESIAN_POINT('Ctrl Pts',(-36.1012716601613,0.364727636112995,
304.824172392622));
#11301=CARTESIAN_POINT('Ctrl Pts',(-36.1130790496947,0.278486353953334,
304.830001347721));
#11302=CARTESIAN_POINT('Ctrl Pts',(-36.1201162049507,0.191711295426038,
304.83583030282));
#11303=CARTESIAN_POINT('Ctrl Pts',(-36.1252509851141,0.128394396338522,
304.840083499165));
#11304=CARTESIAN_POINT('Ctrl Pts',(-36.1278470108903,0.0647937164408854,
304.84433669551));
#11305=CARTESIAN_POINT('Ctrl Pts',(-36.1278767663821,0.00110814072209554,
304.848589891855));
#11306=CARTESIAN_POINT('Ctrl Pts',(-32.6699490795102,2.1084154079953,304.328189117937));
#11307=CARTESIAN_POINT('Ctrl Pts',(-32.6782653702109,2.11269965459836,304.328799546289));
#11308=CARTESIAN_POINT('Ctrl Pts',(-32.6866072203208,2.11693480692552,304.329407472493));
#11309=CARTESIAN_POINT('Ctrl Pts',(-32.7878987226301,2.16760885279292,304.336739064943));
#11310=CARTESIAN_POINT('Ctrl Pts',(-32.8837883696344,2.20794568566654,304.343172787889));
#11311=CARTESIAN_POINT('Ctrl Pts',(-33.0768027562493,2.27459241156353,304.355714762328));
#11312=CARTESIAN_POINT('Ctrl Pts',(-33.1735598338358,2.30127513138037,304.361814774846));
#11313=CARTESIAN_POINT('Ctrl Pts',(-33.3646674478112,2.34114797902569,304.373905913891));
#11314=CARTESIAN_POINT('Ctrl Pts',(-33.4586918873183,2.35494030258137,304.379874473848));
#11315=CARTESIAN_POINT('Ctrl Pts',(-33.5855386775497,2.36582876944276,304.388111412626));
#11316=CARTESIAN_POINT('Ctrl Pts',(-33.6178462020658,2.36793673875129,304.390224760418));
#11317=CARTESIAN_POINT('Ctrl Pts',(-33.673001948259,2.3704029012557,304.393864174224));
#11318=CARTESIAN_POINT('Ctrl Pts',(-33.6958312191092,2.37109342852079,304.395379710148));
#11319=CARTESIAN_POINT('Ctrl Pts',(-33.7395502163077,2.37178403759726,304.398301118135));
#11320=CARTESIAN_POINT('Ctrl Pts',(-33.7604370354269,2.37183803984174,304.399705162552));
#11321=CARTESIAN_POINT('Ctrl Pts',(-33.815716729144,2.37125079020861,304.40344444518));
#11322=CARTESIAN_POINT('Ctrl Pts',(-33.8500985046813,2.37013720905983,304.405794065494));
#11323=CARTESIAN_POINT('Ctrl Pts',(-34.009584074951,2.36149613499397,304.416809794515));
#11324=CARTESIAN_POINT('Ctrl Pts',(-34.1339728372413,2.34480884998278,304.425750364261));
#11325=CARTESIAN_POINT('Ctrl Pts',(-34.3498712971519,2.29821687594208,304.441764539349));
#11326=CARTESIAN_POINT('Ctrl Pts',(-34.4419926339326,2.27242630110686,304.44875944352));
#11327=CARTESIAN_POINT('Ctrl Pts',(-34.6050449406822,2.21595622508672,304.461249137615));
#11328=CARTESIAN_POINT('Ctrl Pts',(-34.6765214481488,2.18723569282459,304.466762553553));
#11329=CARTESIAN_POINT('Ctrl Pts',(-34.7653883985863,2.1463975767723,304.473567401631));
#11330=CARTESIAN_POINT('Ctrl Pts',(-34.7841821124664,2.13745968116715,304.47500346471));
#11331=CARTESIAN_POINT('Ctrl Pts',(-34.8147838799986,2.12240910270798,304.477333941864));
#11332=CARTESIAN_POINT('Ctrl Pts',(-34.8266621392933,2.11644261226328,304.478236558375));
#11333=CARTESIAN_POINT('Ctrl Pts',(-34.8492344342421,2.10486580639192,304.479947140955));
#11334=CARTESIAN_POINT('Ctrl Pts',(-34.8599368787003,2.09927313469282,304.480756200937));
#11335=CARTESIAN_POINT('Ctrl Pts',(-34.8896707540121,2.08344512872126,304.482999673416));
#11336=CARTESIAN_POINT('Ctrl Pts',(-34.9086062511183,2.07303080166268,304.484423452954));
#11337=CARTESIAN_POINT('Ctrl Pts',(-35.0022685373012,2.01983739798276,304.491454615318));
#11338=CARTESIAN_POINT('Ctrl Pts',(-35.0747768219675,1.97326574074742,304.496862236112));
#11339=CARTESIAN_POINT('Ctrl Pts',(-35.262442986556,1.83775374427855,304.511199676449));
#11340=CARTESIAN_POINT('Ctrl Pts',(-35.3722143693567,1.74200713903659,304.519978661525));
#11341=CARTESIAN_POINT('Ctrl Pts',(-35.5273075093886,1.57937256221924,304.534004445851));
#11342=CARTESIAN_POINT('Ctrl Pts',(-35.5791617448385,1.51922365397991,304.539032010844));
#11343=CARTESIAN_POINT('Ctrl Pts',(-35.6467404985982,1.43238258076507,304.546170138496));
#11344=CARTESIAN_POINT('Ctrl Pts',(-35.6651085303727,1.40780987150087,304.548177175332));
#11345=CARTESIAN_POINT('Ctrl Pts',(-35.69613791137,1.36457465464386,304.551691179659));
#11346=CARTESIAN_POINT('Ctrl Pts',(-35.7090195187109,1.34607469175883,304.55318945473));
#11347=CARTESIAN_POINT('Ctrl Pts',(-35.7351778839948,1.30734130836825,304.556317085283));
#11348=CARTESIAN_POINT('Ctrl Pts',(-35.7484125244415,1.28708275278554,304.557947795987));
#11349=CARTESIAN_POINT('Ctrl Pts',(-35.7824705642847,1.23316514691137,304.562276423632));
#11350=CARTESIAN_POINT('Ctrl Pts',(-35.8027646302404,1.19918247371485,304.564993207242));
#11351=CARTESIAN_POINT('Ctrl Pts',(-35.9180435264787,0.994689985837558,
304.581284146611));
#11352=CARTESIAN_POINT('Ctrl Pts',(-35.9925213376725,0.813513936862788,
304.595574591462));
#11353=CARTESIAN_POINT('Ctrl Pts',(-36.0694956912709,0.531886809244084,
304.616846955885));
#11354=CARTESIAN_POINT('Ctrl Pts',(-36.0892866419849,0.436976204739904,
304.623848480326));
#11355=CARTESIAN_POINT('Ctrl Pts',(-36.106351258462,0.319559778493578,304.632124203974));
#11356=CARTESIAN_POINT('Ctrl Pts',(-36.1091867409673,0.297963852824,304.633630371095));
#11357=CARTESIAN_POINT('Ctrl Pts',(-36.1132862741035,0.263017176194256,
304.636038731036));
#11358=CARTESIAN_POINT('Ctrl Pts',(-36.1147352406086,0.249689944196646,
304.63695040773));
#11359=CARTESIAN_POINT('Ctrl Pts',(-36.1173987716898,0.223094788382456,
304.638755264668));
#11360=CARTESIAN_POINT('Ctrl Pts',(-36.1186146846707,0.209827597193498,
304.639648440372));
#11361=CARTESIAN_POINT('Ctrl Pts',(-36.1215173211892,0.174922339337079,
304.6419811052));
#11362=CARTESIAN_POINT('Ctrl Pts',(-36.1230190001543,0.153269499035327,
304.643410757257));
#11363=CARTESIAN_POINT('Ctrl Pts',(-36.1292740403634,0.0407106423377964,
304.650766703633));
#11364=CARTESIAN_POINT('Ctrl Pts',(-36.1290887556011,-0.0504029442347439,
304.656465858657));
#11365=CARTESIAN_POINT('Ctrl Pts',(-36.1152207116063,-0.282784969798882,
304.670847441797));
#11366=CARTESIAN_POINT('Ctrl Pts',(-36.0941094233503,-0.423236087679238,
304.679408260687));
#11367=CARTESIAN_POINT('Ctrl Pts',(-36.0420461705075,-0.637114207728523,
304.693141830167));
#11368=CARTESIAN_POINT('Ctrl Pts',(-36.0197471952671,-0.712293986752316,
304.698105324059));
#11369=CARTESIAN_POINT('Ctrl Pts',(-35.9836997356749,-0.814886906975633,
304.70515745996));
#11370=CARTESIAN_POINT('Ctrl Pts',(-35.9730804372024,-0.84334944200655,
304.707144348249));
#11371=CARTESIAN_POINT('Ctrl Pts',(-35.953717891521,-0.892351010473146,
304.710622477106));
#11372=CARTESIAN_POINT('Ctrl Pts',(-35.9452257807146,-0.912985499309556,
304.712105111559));
#11373=CARTESIAN_POINT('Ctrl Pts',(-35.9270259661663,-0.95549381598129,
304.715198536749));
#11374=CARTESIAN_POINT('Ctrl Pts',(-35.9172758425538,-0.977346591571641,
304.716810649339));
#11375=CARTESIAN_POINT('Ctrl Pts',(-35.8907519089747,-1.03445583109363,
304.721083360992));
#11376=CARTESIAN_POINT('Ctrl Pts',(-35.8734359034383,-1.06945082096291,
304.723762454098));
#11377=CARTESIAN_POINT('Ctrl Pts',(-35.7760425886514,-1.25463366573736,
304.738277710424));
#11378=CARTESIAN_POINT('Ctrl Pts',(-35.6808490184593,-1.39627745376366,
304.750647367382));
#11379=CARTESIAN_POINT('Ctrl Pts',(-35.5174280069754,-1.59060825631539,
304.769206123132));
#11380=CARTESIAN_POINT('Ctrl Pts',(-35.4601495707921,-1.65182453819164,
304.775322501833));
#11381=CARTESIAN_POINT('Ctrl Pts',(-35.365148622022,-1.74314400070019,304.784754506057));
#11382=CARTESIAN_POINT('Ctrl Pts',(-35.3295433634664,-1.7753487714525,304.788147926515));
#11383=CARTESIAN_POINT('Ctrl Pts',(-35.2793972033692,-1.81801104926626,
304.792710540428));
#11384=CARTESIAN_POINT('Ctrl Pts',(-35.2656813164995,-1.82941578158022,
304.79393723571));
#11385=CARTESIAN_POINT('Ctrl Pts',(-35.242056355216,-1.84861324599437,304.796012314442));
#11386=CARTESIAN_POINT('Ctrl Pts',(-35.2322117540529,-1.85648345259635,
304.796865975599));
#11387=CARTESIAN_POINT('Ctrl Pts',(-35.2108176840076,-1.87330902322722,
304.798697060663));
#11388=CARTESIAN_POINT('Ctrl Pts',(-35.1992475669361,-1.88223663214954,
304.799672625231));
#11389=CARTESIAN_POINT('Ctrl Pts',(-35.1660479879882,-1.90736762676136,
304.802432724611));
#11390=CARTESIAN_POINT('Ctrl Pts',(-35.1442223623002,-1.92330961392877,
304.804200509387));
#11391=CARTESIAN_POINT('Ctrl Pts',(-35.0332510231948,-2.0014925185186,304.81298351766));
#11392=CARTESIAN_POINT('Ctrl Pts',(-34.9401636307845,-2.05793111903594,
304.81970156455));
#11393=CARTESIAN_POINT('Ctrl Pts',(-34.687689332789,-2.18818119480047,304.837143681335));
#11394=CARTESIAN_POINT('Ctrl Pts',(-34.5234376639537,-2.25103824517571,
304.847783709351));
#11395=CARTESIAN_POINT('Ctrl Pts',(-34.3165794975337,-2.30490077680979,
304.861515704527));
#11396=CARTESIAN_POINT('Ctrl Pts',(-34.279166141357,-2.31367767379314,304.864009581738));
#11397=CARTESIAN_POINT('Ctrl Pts',(-34.2181698420588,-2.32643190467913,
304.868101127832));
#11398=CARTESIAN_POINT('Ctrl Pts',(-34.1947101383066,-2.33096841556767,
304.86968083311));
#11399=CARTESIAN_POINT('Ctrl Pts',(-34.1490178393951,-2.33908996220453,
304.872771351299));
#11400=CARTESIAN_POINT('Ctrl Pts',(-34.1267947776484,-2.34271432315199,
304.874280728407));
#11401=CARTESIAN_POINT('Ctrl Pts',(-34.0738119598627,-2.35058256274346,
304.877895701483));
#11402=CARTESIAN_POINT('Ctrl Pts',(-34.0430145325771,-2.35453976404966,
304.880010104894));
#11403=CARTESIAN_POINT('Ctrl Pts',(-33.92933447257,-2.36688327460594,304.887866950756));
#11404=CARTESIAN_POINT('Ctrl Pts',(-33.8461125575706,-2.37150523017019,
304.893723152976));
#11405=CARTESIAN_POINT('Ctrl Pts',(-33.5997387028622,-2.37220130939454,
304.911349754175));
#11406=CARTESIAN_POINT('Ctrl Pts',(-33.4370407070916,-2.35583818044118,
304.923395833102));
#11407=CARTESIAN_POINT('Ctrl Pts',(-33.2130306411181,-2.30966540822406,
304.939917123234));
#11408=CARTESIAN_POINT('Ctrl Pts',(-33.1493041784252,-2.29374706224781,
304.944603642607));
#11409=CARTESIAN_POINT('Ctrl Pts',(-33.0668620024144,-2.26947637416521,
304.950583508467));
#11410=CARTESIAN_POINT('Ctrl Pts',(-33.0474822819601,-2.2634999408469,304.951983013864));
#11411=CARTESIAN_POINT('Ctrl Pts',(-33.0169692056857,-2.2536598129924,304.954174142535));
#11412=CARTESIAN_POINT('Ctrl Pts',(-33.0057843972445,-2.24996061983072,
304.954974665781));
#11413=CARTESIAN_POINT('Ctrl Pts',(-32.9819992704595,-2.24189698191096,
304.956670663574));
#11414=CARTESIAN_POINT('Ctrl Pts',(-32.969407203646,-2.23750928501221,304.957564693609));
#11415=CARTESIAN_POINT('Ctrl Pts',(-32.9365109384593,-2.22573455791831,
304.959891866302));
#11416=CARTESIAN_POINT('Ctrl Pts',(-32.916268961524,-2.21817568436677,304.961315355593));
#11417=CARTESIAN_POINT('Ctrl Pts',(-32.808597695364,-2.17628317470362,304.968856047782));
#11418=CARTESIAN_POINT('Ctrl Pts',(-32.723153164064,-2.13705154587898,304.974731095106));
#11419=CARTESIAN_POINT('Ctrl Pts',(-32.4636178993085,-1.99867148540465,
304.992892552078));
#11420=CARTESIAN_POINT('Ctrl Pts',(-32.299630193214,-1.88251978712095,305.004913331659));
#11421=CARTESIAN_POINT('Ctrl Pts',(-32.1238352068006,-1.72113390130632,
305.020243514319));
#11422=CARTESIAN_POINT('Ctrl Pts',(-32.0961303474466,-1.69442888492212,
305.022740644329));
#11423=CARTESIAN_POINT('Ctrl Pts',(-32.0522926497168,-1.65006590312639,
305.026835639484));
#11424=CARTESIAN_POINT('Ctrl Pts',(-32.0357551809641,-1.63281649643271,
305.028415464109));
#11425=CARTESIAN_POINT('Ctrl Pts',(-32.0041593565324,-1.59884754969592,
305.031504857571));
#11426=CARTESIAN_POINT('Ctrl Pts',(-31.9890726985927,-1.58215774991069,
305.033012971713));
#11427=CARTESIAN_POINT('Ctrl Pts',(-31.953775998309,-1.54197569274489,305.036622484181));
#11428=CARTESIAN_POINT('Ctrl Pts',(-31.933784918249,-1.51829751615685,305.038732638446));
#11429=CARTESIAN_POINT('Ctrl Pts',(-31.8621103250249,-1.4299481424619,305.046549360928));
#11430=CARTESIAN_POINT('Ctrl Pts',(-31.8133637656336,-1.36298169787433,
305.052368260065));
#11431=CARTESIAN_POINT('Ctrl Pts',(-31.6808390316945,-1.15932954321583,
305.069749601049));
#11432=CARTESIAN_POINT('Ctrl Pts',(-31.6072905546142,-1.01654331702153,
305.08157710485));
#11433=CARTESIAN_POINT('Ctrl Pts',(-31.5233622624702,-0.80296940239596,
305.09818044733));
#11434=CARTESIAN_POINT('Ctrl Pts',(-31.5008572958237,-0.737399886432819,
305.103135582619));
#11435=CARTESIAN_POINT('Ctrl Pts',(-31.4754326355699,-0.651194797441105,
305.109393110757));
#11436=CARTESIAN_POINT('Ctrl Pts',(-31.4698679923482,-0.631380448433861,
305.110814094916));
#11437=CARTESIAN_POINT('Ctrl Pts',(-31.4615135451354,-0.600072342127738,
305.113029528886));
#11438=CARTESIAN_POINT('Ctrl Pts',(-31.4585507307447,-0.588626388530102,
305.113833241256));
#11439=CARTESIAN_POINT('Ctrl Pts',(-31.4524527635835,-0.564320948919424,
305.115526047765));
#11440=CARTESIAN_POINT('Ctrl Pts',(-31.4493394143139,-0.551456410201613,
305.116413804899));
#11441=CARTESIAN_POINT('Ctrl Pts',(-31.4415242031187,-0.517938668691449,
305.118707071989));
#11442=CARTESIAN_POINT('Ctrl Pts',(-31.4369908902023,-0.497246773233944,
305.120103415336));
#11443=CARTESIAN_POINT('Ctrl Pts',(-31.4155611911165,-0.392755688942494,
305.127070252656));
#11444=CARTESIAN_POINT('Ctrl Pts',(-31.402925106527,-0.308138556682372,
305.132440566156));
#11445=CARTESIAN_POINT('Ctrl Pts',(-31.3774455707182,-0.0383664983175095,
305.149221959223));
#11446=CARTESIAN_POINT('Ctrl Pts',(-31.3817245529169,0.147682064217546,
305.160345323115));
#11447=CARTESIAN_POINT('Ctrl Pts',(-31.4148545678939,0.38250795782754,305.175390393175));
#11448=CARTESIAN_POINT('Ctrl Pts',(-31.4237447799637,0.433429934434157,
305.178710369656));
#11449=CARTESIAN_POINT('Ctrl Pts',(-31.4397470918975,0.510193066831521,
305.183826441513));
#11450=CARTESIAN_POINT('Ctrl Pts',(-31.4456456356672,0.536272890233299,
305.185584278798));
#11451=CARTESIAN_POINT('Ctrl Pts',(-31.4572069649306,0.58365238906946,305.188816687164));
#11452=CARTESIAN_POINT('Ctrl Pts',(-31.4627281982615,0.604983734482728,
305.190286538057));
#11453=CARTESIAN_POINT('Ctrl Pts',(-31.4754843913659,0.651581025985171,
305.193530857604));
#11454=CARTESIAN_POINT('Ctrl Pts',(-31.4828436418333,0.676809588065451,
305.195309214568));
#11455=CARTESIAN_POINT('Ctrl Pts',(-31.5056773284675,0.750508331398769,
305.200570982667));
#11456=CARTESIAN_POINT('Ctrl Pts',(-31.5222931237489,0.798606291818543,
305.204090964883));
#11457=CARTESIAN_POINT('Ctrl Pts',(-31.5649753820951,0.910374560957247,
305.212479071801));
#11458=CARTESIAN_POINT('Ctrl Pts',(-31.5922898892316,0.973516730120223,
305.217382473062));
#11459=CARTESIAN_POINT('Ctrl Pts',(-31.661963929818,1.11710852273795,305.228896027504));
#11460=CARTESIAN_POINT('Ctrl Pts',(-31.7062826271992,1.19648953636735,305.235541049883));
#11461=CARTESIAN_POINT('Ctrl Pts',(-31.8104008333537,1.36014086664721,305.249702610231));
#11462=CARTESIAN_POINT('Ctrl Pts',(-31.8713805152212,1.44345694112722,305.257201538312));
#11463=CARTESIAN_POINT('Ctrl Pts',(-31.9546956097464,1.54296872142631,305.266318056573));
#11464=CARTESIAN_POINT('Ctrl Pts',(-31.9721393401096,1.56310450938407,305.268171349892));
#11465=CARTESIAN_POINT('Ctrl Pts',(-31.9996158306984,1.59376207571798,305.271000981311));
#11466=CARTESIAN_POINT('Ctrl Pts',(-32.0094116937441,1.60449204085024,305.271992878348));
#11467=CARTESIAN_POINT('Ctrl Pts',(-32.0279391648847,1.62441543461217,305.273836412733));
#11468=CARTESIAN_POINT('Ctrl Pts',(-32.036646388413,1.63362943530695,305.274689588707));
#11469=CARTESIAN_POINT('Ctrl Pts',(-32.0579744418754,1.65583936331158,305.276748532716));
#11470=CARTESIAN_POINT('Ctrl Pts',(-32.070670983612,1.66876126982694,305.277948572669));
#11471=CARTESIAN_POINT('Ctrl Pts',(-32.1187828322008,1.71661776585652,305.282406991744));
#11472=CARTESIAN_POINT('Ctrl Pts',(-32.1551486507734,1.7505832150299,305.285599973393));
#11473=CARTESIAN_POINT('Ctrl Pts',(-32.2594639823441,1.84204097850255,305.294371113383));
#11474=CARTESIAN_POINT('Ctrl Pts',(-32.3296216069873,1.89689206971494,305.299839352546));
#11475=CARTESIAN_POINT('Ctrl Pts',(-32.4882142663704,2.00709720902461,305.311679881417));
#11476=CARTESIAN_POINT('Ctrl Pts',(-32.5774941016077,2.06078602681652,305.318033273464));
#11477=CARTESIAN_POINT('Ctrl Pts',(-32.6699493942465,2.1084155701358,305.324530114841));
#11478=CARTESIAN_POINT('Origin',(-33.7561270252576,0.,302.151410108095));
#11479=CARTESIAN_POINT('',(-32.669949078383,2.10841540741462,306.520649966606));
#11480=CARTESIAN_POINT('',(-32.6699490794746,2.10841540797695,306.325637667994));
#11481=CARTESIAN_POINT('',(-32.6699490794746,2.10841540797695,302.151410108095));
#11482=CARTESIAN_POINT('Ctrl Pts',(-32.669949078383,2.10841540741463,306.520649966606));
#11483=CARTESIAN_POINT('Ctrl Pts',(-32.5859421857569,2.06513815102808,306.514515728316));
#11484=CARTESIAN_POINT('Ctrl Pts',(-32.5045827081745,2.0168715384183,306.508627603963));
#11485=CARTESIAN_POINT('Ctrl Pts',(-32.3148472989697,1.88839381620105,306.494506776106));
#11486=CARTESIAN_POINT('Ctrl Pts',(-32.2100159536117,1.80356823753118,306.486354837066));
#11487=CARTESIAN_POINT('Ctrl Pts',(-32.0577711477892,1.65729893463586,306.473166477512));
#11488=CARTESIAN_POINT('Ctrl Pts',(-32.0051979229085,1.60165476444168,306.46831540019));
#11489=CARTESIAN_POINT('Ctrl Pts',(-31.9357357856755,1.52062077854595,306.461390413495));
#11490=CARTESIAN_POINT('Ctrl Pts',(-31.9165040328186,1.49729720699368,306.459412475234));
#11491=CARTESIAN_POINT('Ctrl Pts',(-31.8838222108656,1.45608151120502,306.455939009056));
#11492=CARTESIAN_POINT('Ctrl Pts',(-31.8701696527893,1.43835441249426,306.454451825248));
#11493=CARTESIAN_POINT('Ctrl Pts',(-31.8423003634598,1.40108862068816,306.451337805631));
#11494=CARTESIAN_POINT('Ctrl Pts',(-31.828127392355,1.38152059509149,306.449709489951));
#11495=CARTESIAN_POINT('Ctrl Pts',(-31.7913812743704,1.32911983763755,306.445365087293));
#11496=CARTESIAN_POINT('Ctrl Pts',(-31.7693331422192,1.29593022202604,306.442629595394));
#11497=CARTESIAN_POINT('Ctrl Pts',(-31.6628690667612,1.12656021743971,306.428742083711));
#11498=CARTESIAN_POINT('Ctrl Pts',(-31.5915825217937,0.982648453125285,
306.417129796858));
#11499=CARTESIAN_POINT('Ctrl Pts',(-31.5041518157228,0.749468535102951,
306.398939522738));
#11500=CARTESIAN_POINT('Ctrl Pts',(-31.4776521538253,0.664566837404724,
306.392444829981));
#11501=CARTESIAN_POINT('Ctrl Pts',(-31.4438573478665,0.530167777379962,
306.382518418221));
#11502=CARTESIAN_POINT('Ctrl Pts',(-31.4332530967946,0.481587413090841,
306.379001225183));
#11503=CARTESIAN_POINT('Ctrl Pts',(-31.4208787636503,0.414899514617037,
306.374299549399));
#11504=CARTESIAN_POINT('Ctrl Pts',(-31.4177785956699,0.397055063656548,
306.373053721082));
#11505=CARTESIAN_POINT('Ctrl Pts',(-31.4128559983261,0.366660216980718,
306.37095443548));
#11506=CARTESIAN_POINT('Ctrl Pts',(-31.4109293093348,0.354127836868415,
306.370095456937));
#11507=CARTESIAN_POINT('Ctrl Pts',(-31.4070088490947,0.327190017686873,
306.368263792683));
#11508=CARTESIAN_POINT('Ctrl Pts',(-31.4050469147632,0.312780841765095,
306.367292825615));
#11509=CARTESIAN_POINT('Ctrl Pts',(-31.399862068979,0.271891595838558,306.364560059864));
#11510=CARTESIAN_POINT('Ctrl Pts',(-31.3969530595573,0.245373041082243,
306.362814491902));
#11511=CARTESIAN_POINT('Ctrl Pts',(-31.3849179393402,0.115476789763453,
306.354369901795));
#11512=CARTESIAN_POINT('Ctrl Pts',(-31.3821352098135,0.0116152235876252,
306.347941672039));
#11513=CARTESIAN_POINT('Ctrl Pts',(-31.3900120649434,-0.191066256825405,
306.335476703579));
#11514=CARTESIAN_POINT('Ctrl Pts',(-31.4000526275048,-0.289688486745452,
306.329446993958));
#11515=CARTESIAN_POINT('Ctrl Pts',(-31.4266668977316,-0.450441557810462,
306.31935132944));
#11516=CARTESIAN_POINT('Ctrl Pts',(-31.4396484641922,-0.513038324383106,
306.315352856988));
#11517=CARTESIAN_POINT('Ctrl Pts',(-31.4668583446621,-0.62191852468309,
306.308209808261));
#11518=CARTESIAN_POINT('Ctrl Pts',(-31.4800053625378,-0.668433549038073,
306.305096555846));
#11519=CARTESIAN_POINT('Ctrl Pts',(-31.50234046248,-0.739128291225599,306.300250648081));
#11520=CARTESIAN_POINT('Ctrl Pts',(-31.5105187371391,-0.763614975167525,
306.298550766854));
#11521=CARTESIAN_POINT('Ctrl Pts',(-31.5264254856782,-0.808774368515765,
306.295373301665));
#11522=CARTESIAN_POINT('Ctrl Pts',(-31.5340460137308,-0.829482282058013,
306.293899449051));
#11523=CARTESIAN_POINT('Ctrl Pts',(-31.5517420555133,-0.875574512768605,
306.290579590689));
#11524=CARTESIAN_POINT('Ctrl Pts',(-31.5619691863605,-0.900896826129921,
306.288728641907));
#11525=CARTESIAN_POINT('Ctrl Pts',(-31.589682078915,-0.966240930140267,
306.283879195033));
#11526=CARTESIAN_POINT('Ctrl Pts',(-31.6078394096627,-1.00596477487028,
306.28085854264));
#11527=CARTESIAN_POINT('Ctrl Pts',(-31.7181771697776,-1.23072794960111,
306.263339490632));
#11528=CARTESIAN_POINT('Ctrl Pts',(-31.8331349176203,-1.4035688354149,306.248063092413));
#11529=CARTESIAN_POINT('Ctrl Pts',(-32.0013349112842,-1.59634644848115,
306.229536840458));
#11530=CARTESIAN_POINT('Ctrl Pts',(-32.0348189527007,-1.63239591537284,
306.226002855252));
#11531=CARTESIAN_POINT('Ctrl Pts',(-32.0932396475318,-1.69149442552852,
306.220122446263));
#11532=CARTESIAN_POINT('Ctrl Pts',(-32.117593537376,-1.71509653322599,306.217748884753));
#11533=CARTESIAN_POINT('Ctrl Pts',(-32.1539925043496,-1.74888857310092,
306.214323717282));
#11534=CARTESIAN_POINT('Ctrl Pts',(-32.1656452705347,-1.75949256517752,
306.213244854934));
#11535=CARTESIAN_POINT('Ctrl Pts',(-32.1867381937233,-1.77830628013019,
306.211324776825));
#11536=CARTESIAN_POINT('Ctrl Pts',(-32.1961386417187,-1.78655836460439,
306.210480600691));
#11537=CARTESIAN_POINT('Ctrl Pts',(-32.2177381344329,-1.8052187640216,306.208566813081));
#11538=CARTESIAN_POINT('Ctrl Pts',(-32.2299780242117,-1.81557826269784,
306.207500654272));
#11539=CARTESIAN_POINT('Ctrl Pts',(-32.270451754839,-1.84913553923771,306.20403115786));
#11540=CARTESIAN_POINT('Ctrl Pts',(-32.2991181019938,-1.87180623836152,
306.201661702312));
#11541=CARTESIAN_POINT('Ctrl Pts',(-32.4843618834289,-2.01147006895618,
306.18681524043));
#11542=CARTESIAN_POINT('Ctrl Pts',(-32.6543842624245,-2.10940218869972,
306.175192372596));
#11543=CARTESIAN_POINT('Ctrl Pts',(-32.9163109393161,-2.21986215564156,
306.157537639525));
#11544=CARTESIAN_POINT('Ctrl Pts',(-32.9999738185638,-2.24973528604135,
306.151941586505));
#11545=CARTESIAN_POINT('Ctrl Pts',(-33.115442501059,-2.28379544737745,306.144145635967));
#11546=CARTESIAN_POINT('Ctrl Pts',(-33.1459516339184,-2.29213527986041,
306.142079543677));
#11547=CARTESIAN_POINT('Ctrl Pts',(-33.1985263609063,-2.30538284176792,
306.138503552515));
#11548=CARTESIAN_POINT('Ctrl Pts',(-33.2205125595828,-2.31058988832539,
306.137003503662));
#11549=CARTESIAN_POINT('Ctrl Pts',(-33.2656822936358,-2.3206082228344,306.133910656441));
#11550=CARTESIAN_POINT('Ctrl Pts',(-33.2888701246602,-2.32538802713199,
306.132317033865));
#11551=CARTESIAN_POINT('Ctrl Pts',(-33.3488620444505,-2.3368209025973,306.128177011067));
#11552=CARTESIAN_POINT('Ctrl Pts',(-33.3857576886613,-2.34295176486046,
306.12561439901));
#11553=CARTESIAN_POINT('Ctrl Pts',(-33.6262365606258,-2.37708957125409,
306.108796088669));
#11554=CARTESIAN_POINT('Ctrl Pts',(-33.8325529476159,-2.37940197182712,
306.093720019455));
#11555=CARTESIAN_POINT('Ctrl Pts',(-34.126972502786,-2.34434797367796,306.072136042513));
#11556=CARTESIAN_POINT('Ctrl Pts',(-34.2167289645676,-2.32837776913838,
306.065565053226));
#11557=CARTESIAN_POINT('Ctrl Pts',(-34.3262375765445,-2.30231034737386,
306.057716543538));
#11558=CARTESIAN_POINT('Ctrl Pts',(-34.3470553956057,-2.29705522775395,
306.056232348312));
#11559=CARTESIAN_POINT('Ctrl Pts',(-34.380648899234,-2.28808814338242,306.053853128423));
#11560=CARTESIAN_POINT('Ctrl Pts',(-34.393469273889,-2.28455024130282,306.052948901362));
#11561=CARTESIAN_POINT('Ctrl Pts',(-34.4191540553746,-2.27722923611528,
306.05114584765));
#11562=CARTESIAN_POINT('Ctrl Pts',(-34.4320174715421,-2.27344451513548,
306.050247145231));
#11563=CARTESIAN_POINT('Ctrl Pts',(-34.4658856509404,-2.2631668238753,306.047890616694));
#11564=CARTESIAN_POINT('Ctrl Pts',(-34.486833965104,-2.25649037965162,306.046442918235));
#11565=CARTESIAN_POINT('Ctrl Pts',(-34.6047302456006,-2.21710151706872,
306.038335284188));
#11566=CARTESIAN_POINT('Ctrl Pts',(-34.6995855484716,-2.17843006281214,
306.031963474114));
#11567=CARTESIAN_POINT('Ctrl Pts',(-34.9113097101002,-2.07567823304051,
306.01746871856));
#11568=CARTESIAN_POINT('Ctrl Pts',(-35.0258636949191,-2.00764917148078,
306.009410003655));
#11569=CARTESIAN_POINT('Ctrl Pts',(-35.196016047125,-1.88618734452235,305.996347629565));
#11570=CARTESIAN_POINT('Ctrl Pts',(-35.2557542629721,-1.83904853898069,
305.991524295012));
#11571=CARTESIAN_POINT('Ctrl Pts',(-35.3358804164165,-1.76931839192646,
305.984631950444));
#11572=CARTESIAN_POINT('Ctrl Pts',(-35.3582589062801,-1.74908022929873,
305.982657633036));
#11573=CARTESIAN_POINT('Ctrl Pts',(-35.3965439850316,-1.71310551705073,
305.979188325287));
#11574=CARTESIAN_POINT('Ctrl Pts',(-35.4126255547623,-1.69756027218825,
305.977701618089));
#11575=CARTESIAN_POINT('Ctrl Pts',(-35.4456331837544,-1.66473777929286,
305.974586456959));
#11576=CARTESIAN_POINT('Ctrl Pts',(-35.4625195510671,-1.64742447649363,
305.972956493689));
#11577=CARTESIAN_POINT('Ctrl Pts',(-35.5065962991275,-1.60082853033872,
305.968602387761));
#11578=CARTESIAN_POINT('Ctrl Pts',(-35.5333154085814,-1.57111290976394,
305.965858683439));
#11579=CARTESIAN_POINT('Ctrl Pts',(-35.6620786772266,-1.42041983279592,
305.952097224956));
#11580=CARTESIAN_POINT('Ctrl Pts',(-35.7525707753658,-1.29013223060072,
305.940632188562));
#11581=CARTESIAN_POINT('Ctrl Pts',(-35.8731574278445,-1.07307810265468,
305.922495958677));
#11582=CARTESIAN_POINT('Ctrl Pts',(-35.9123886869014,-0.991892828689847,
305.91590960323));
#11583=CARTESIAN_POINT('Ctrl Pts',(-35.9661029843121,-0.862388936626612,
305.905864771686));
#11584=CARTESIAN_POINT('Ctrl Pts',(-35.9838289698564,-0.815507983326928,
305.902318764643));
#11585=CARTESIAN_POINT('Ctrl Pts',(-36.0059387625847,-0.750916096054525,
305.89758579372));
#11586=CARTESIAN_POINT('Ctrl Pts',(-36.0116225368572,-0.733667421540767,
305.896336474399));
#11587=CARTESIAN_POINT('Ctrl Pts',(-36.0209395089188,-0.704260898569048,
305.894233216038));
#11588=CARTESIAN_POINT('Ctrl Pts',(-36.0246741966852,-0.692136375137347,
305.893373702854));
#11589=CARTESIAN_POINT('Ctrl Pts',(-36.0324735993946,-0.666074373641117,
305.891543112385));
#11590=CARTESIAN_POINT('Ctrl Pts',(-36.0365079058945,-0.652128717041853,
305.890573722865));
#11591=CARTESIAN_POINT('Ctrl Pts',(-36.0475598094166,-0.612567704092598,
305.887850082289));
#11592=CARTESIAN_POINT('Ctrl Pts',(-36.0542758042908,-0.586869431616941,
305.886111893029));
#11593=CARTESIAN_POINT('Ctrl Pts',(-36.0844985742969,-0.46273652068267,
305.877840317001));
#11594=CARTESIAN_POINT('Ctrl Pts',(-36.102123109679,-0.362968171454786,
305.87156408442));
#11595=CARTESIAN_POINT('Ctrl Pts',(-36.1229431829177,-0.1759154587442,305.859991865556));
#11596=CARTESIAN_POINT('Ctrl Pts',(-36.127802440045,-0.0889980115911998,
305.854690997065));
#11597=CARTESIAN_POINT('Ctrl Pts',(-36.1279659246806,0.103875004344682,
305.842791052475));
#11598=CARTESIAN_POINT('Ctrl Pts',(-36.120965002638,0.209636290981643,305.836170916785));
#11599=CARTESIAN_POINT('Ctrl Pts',(-36.1024399490108,0.348075470535023,
305.827151216386));
#11600=CARTESIAN_POINT('Ctrl Pts',(-36.0972406204719,0.381481081768892,
305.824947854604));
#11601=CARTESIAN_POINT('Ctrl Pts',(-36.0877118767881,0.435129918978208,
305.821359939336));
#11602=CARTESIAN_POINT('Ctrl Pts',(-36.0838282154977,0.455448229044223,
305.819989606697));
#11603=CARTESIAN_POINT('Ctrl Pts',(-36.0751208952325,0.497977929059514,
305.817095739372));
#11604=CARTESIAN_POINT('Ctrl Pts',(-36.070242749057,0.520175875309198,305.815570589025));
#11605=CARTESIAN_POINT('Ctrl Pts',(-36.057636892539,0.57384714034288,305.811845586991));
#11606=CARTESIAN_POINT('Ctrl Pts',(-36.0495818343527,0.605238024917801,
305.80963542613));
#11607=CARTESIAN_POINT('Ctrl Pts',(-36.0148728685773,0.729837443919163,
305.800731698052));
#11608=CARTESIAN_POINT('Ctrl Pts',(-35.9831617782423,0.821527477216697,
305.793879083827));
#11609=CARTESIAN_POINT('Ctrl Pts',(-35.9086552771279,1.00061965048489,305.779915052783));
#11610=CARTESIAN_POINT('Ctrl Pts',(-35.8659122748551,1.0878520503058,305.772816392382));
#11611=CARTESIAN_POINT('Ctrl Pts',(-35.7669961863955,1.26183644752888,305.758205094667));
#11612=CARTESIAN_POINT('Ctrl Pts',(-35.7102502153142,1.34804759267916,305.750709294088));
#11613=CARTESIAN_POINT('Ctrl Pts',(-35.6320043772519,1.45154808598281,305.74159551184));
#11614=CARTESIAN_POINT('Ctrl Pts',(-35.6155819954625,1.47252675604757,305.739742170307));
#11615=CARTESIAN_POINT('Ctrl Pts',(-35.5896585178091,1.50451705174639,305.736912108734));
#11616=CARTESIAN_POINT('Ctrl Pts',(-35.5804043233681,1.51572479714362,305.735919842129));
#11617=CARTESIAN_POINT('Ctrl Pts',(-35.5628833161761,1.53655152698258,305.734075669588));
#11618=CARTESIAN_POINT('Ctrl Pts',(-35.5546419090117,1.54618986876182,305.733222224587));
#11619=CARTESIAN_POINT('Ctrl Pts',(-35.5344335987826,1.56944331605833,305.731162297081));
#11620=CARTESIAN_POINT('Ctrl Pts',(-35.5223872628351,1.58298812865255,305.729961551632));
#11621=CARTESIAN_POINT('Ctrl Pts',(-35.4766481660143,1.6332445747544,305.725497050351));
#11622=CARTESIAN_POINT('Ctrl Pts',(-35.4419542858273,1.66903207742966,305.722298922237));
#11623=CARTESIAN_POINT('Ctrl Pts',(-35.3420568664534,1.76578231552372,305.713507004709));
#11624=CARTESIAN_POINT('Ctrl Pts',(-35.2745011740597,1.8241991677095,305.70802375722));
#11625=CARTESIAN_POINT('Ctrl Pts',(-35.0773840899219,1.97609527084552,305.692766908467));
#11626=CARTESIAN_POINT('Ctrl Pts',(-34.9414605609438,2.06049773492288,305.683032317465));
#11627=CARTESIAN_POINT('Ctrl Pts',(-34.7622727107826,2.14812926176825,305.670237655195));
#11628=CARTESIAN_POINT('Ctrl Pts',(-34.7260131489033,2.16474226498263,305.667652552869));
#11629=CARTESIAN_POINT('Ctrl Pts',(-34.6671345593397,2.18994234155288,305.663450776848));
#11630=CARTESIAN_POINT('Ctrl Pts',(-34.6447721295119,2.19911163713332,305.661854035819));
#11631=CARTESIAN_POINT('Ctrl Pts',(-34.6014474687311,2.21610737808209,305.658756758572));
#11632=CARTESIAN_POINT('Ctrl Pts',(-34.580506868106,2.22398209944306,305.657258049911));
#11633=CARTESIAN_POINT('Ctrl Pts',(-34.5310348788136,2.24179135665439,305.653711934233));
#11634=CARTESIAN_POINT('Ctrl Pts',(-34.5024194583771,2.25147909722816,305.651656585735));
#11635=CARTESIAN_POINT('Ctrl Pts',(-34.4008424240668,2.28371879329282,305.644342255474));
#11636=CARTESIAN_POINT('Ctrl Pts',(-34.3269913489357,2.30328921303756,305.638989361777));
#11637=CARTESIAN_POINT('Ctrl Pts',(-34.1212199201884,2.34731387183811,305.623986341933));
#11638=CARTESIAN_POINT('Ctrl Pts',(-33.9879743762071,2.36419466518143,305.61416025456));
#11639=CARTESIAN_POINT('Ctrl Pts',(-33.7532529304969,2.373892011994,305.597029142096));
#11640=CARTESIAN_POINT('Ctrl Pts',(-33.6523014203619,2.37162306320335,305.589724855603));
#11641=CARTESIAN_POINT('Ctrl Pts',(-33.5298977624896,2.3610381898577,305.581152138852));
#11642=CARTESIAN_POINT('Ctrl Pts',(-33.5080296976663,2.35884056619412,305.579631883657));
#11643=CARTESIAN_POINT('Ctrl Pts',(-33.4728752308131,2.35481341321378,305.577209494369));
#11644=CARTESIAN_POINT('Ctrl Pts',(-33.4595688447433,2.35317467649675,305.576297575623));
#11645=CARTESIAN_POINT('Ctrl Pts',(-33.4330896461668,2.34968547491862,305.574493784921));
#11646=CARTESIAN_POINT('Ctrl Pts',(-33.419917113684,2.34783685433853,305.573601861113));
#11647=CARTESIAN_POINT('Ctrl Pts',(-33.3855170966082,2.34271373261797,305.571285098924));
#11648=CARTESIAN_POINT('Ctrl Pts',(-33.364316755256,2.33926145292947,305.569869775426));
#11649=CARTESIAN_POINT('Ctrl Pts',(-33.2532968417066,2.31963115943838,305.562509799265));
#11650=CARTESIAN_POINT('Ctrl Pts',(-33.1644098621672,2.29856508625893,305.556793753889));
#11651=CARTESIAN_POINT('Ctrl Pts',(-32.9363808009395,2.23041226216226,305.542085719435));
#11652=CARTESIAN_POINT('Ctrl Pts',(-32.8001418803171,2.1754859432645,305.533235699134));
#11653=CARTESIAN_POINT('Ctrl Pts',(-32.6699490731214,2.10841540470401,305.524079281032));
#11654=CARTESIAN_POINT('',(-36.1278766586888,0.00131864288668422,305.651410108095));
#11655=CARTESIAN_POINT('Ctrl Pts',(-32.6699493942465,2.1084155701358,305.324530114841));
#11656=CARTESIAN_POINT('Ctrl Pts',(-32.7195768807531,2.13398181357011,305.328017442592));
#11657=CARTESIAN_POINT('Ctrl Pts',(-32.7701193673887,2.15780226145263,305.331544844162));
#11658=CARTESIAN_POINT('Ctrl Pts',(-32.8581171958471,2.19553294598891,305.33768650562));
#11659=CARTESIAN_POINT('Ctrl Pts',(-32.8951363359132,2.21031249032801,305.340270124394));
#11660=CARTESIAN_POINT('Ctrl Pts',(-32.9551696417961,2.23254322985126,305.344470151115));
#11661=CARTESIAN_POINT('Ctrl Pts',(-32.9779568722895,2.24058767821185,305.346066661418));
#11662=CARTESIAN_POINT('Ctrl Pts',(-33.0220727349457,2.25540750425207,305.349163938566));
#11663=CARTESIAN_POINT('Ctrl Pts',(-33.0433822310108,2.26223197533106,305.350662884598));
#11664=CARTESIAN_POINT('Ctrl Pts',(-33.0936966447019,2.27756395891887,305.354210295848));
#11665=CARTESIAN_POINT('Ctrl Pts',(-33.12277335312,2.28582032858097,305.356266716568));
#11666=CARTESIAN_POINT('Ctrl Pts',(-33.2259568644129,2.31299956258742,305.363590255575));
#11667=CARTESIAN_POINT('Ctrl Pts',(-33.3008061838628,2.32888988597712,305.368951590077));
#11668=CARTESIAN_POINT('Ctrl Pts',(-33.509063948275,2.36267900777135,305.383994759033));
#11669=CARTESIAN_POINT('Ctrl Pts',(-33.6434255365436,2.37288537119634,305.393853831767));
#11670=CARTESIAN_POINT('Ctrl Pts',(-33.8781237761705,2.37072938042785,305.41096735164));
#11671=CARTESIAN_POINT('Ctrl Pts',(-33.9781856953145,2.36345828355269,305.418222840254));
#11672=CARTESIAN_POINT('Ctrl Pts',(-34.0992646054196,2.34689952656979,305.426749717038));
#11673=CARTESIAN_POINT('Ctrl Pts',(-34.1209915457414,2.34362001095034,305.428269590526));
#11674=CARTESIAN_POINT('Ctrl Pts',(-34.1558978222545,2.33785395229119,305.430691603334));
#11675=CARTESIAN_POINT('Ctrl Pts',(-34.169106564501,2.33555683188511,305.431603517906));
#11676=CARTESIAN_POINT('Ctrl Pts',(-34.1953817134525,2.3307574612693,305.433407411194));
#11677=CARTESIAN_POINT('Ctrl Pts',(-34.208447926001,2.32825704056831,305.43429943965));
#11678=CARTESIAN_POINT('Ctrl Pts',(-34.2425615476118,2.32143084862783,305.436616876364));
#11679=CARTESIAN_POINT('Ctrl Pts',(-34.2635729825365,2.31692865894822,305.438032759862));
#11680=CARTESIAN_POINT('Ctrl Pts',(-34.3736798250611,2.29176591605543,305.445405903074));
#11681=CARTESIAN_POINT('Ctrl Pts',(-34.4615957309223,2.26624803299343,305.451133574464));
#11682=CARTESIAN_POINT('Ctrl Pts',(-34.7408377638245,2.16736421187913,305.469439474914));
#11683=CARTESIAN_POINT('Ctrl Pts',(-34.9241705581056,2.07431766408141,305.481717622589));
#11684=CARTESIAN_POINT('Ctrl Pts',(-35.1242853600399,1.93771784646349,305.497297234415));
#11685=CARTESIAN_POINT('Ctrl Pts',(-35.1547861086452,1.91581841452697,305.499735793412));
#11686=CARTESIAN_POINT('Ctrl Pts',(-35.2036736582598,1.87892752774865,305.503759018806));
#11687=CARTESIAN_POINT('Ctrl Pts',(-35.2223786762482,1.86436743602134,305.505326837107));
#11688=CARTESIAN_POINT('Ctrl Pts',(-35.2584678116655,1.83539640179127,305.508409952337));
#11689=CARTESIAN_POINT('Ctrl Pts',(-35.2758705904157,1.82101269222123,305.509924047344));
#11690=CARTESIAN_POINT('Ctrl Pts',(-35.3170782708204,1.78595166804947,305.513577148768));
#11691=CARTESIAN_POINT('Ctrl Pts',(-35.3406808016547,1.76504428104584,305.515725505224));
#11692=CARTESIAN_POINT('Ctrl Pts',(-35.428436535069,1.68413024192097,305.52393295459));
#11693=CARTESIAN_POINT('Ctrl Pts',(-35.4896491678435,1.62105258684898,305.530120152592));
#11694=CARTESIAN_POINT('Ctrl Pts',(-35.6709507099456,1.41218872643857,305.549953012934));
#11695=CARTESIAN_POINT('Ctrl Pts',(-35.777215392898,1.2553971505819,305.563985155322));
#11696=CARTESIAN_POINT('Ctrl Pts',(-35.8826613653697,1.05106930596526,305.580369580621));
#11697=CARTESIAN_POINT('Ctrl Pts',(-35.9005971175389,1.01397410522387,305.583271377605));
#11698=CARTESIAN_POINT('Ctrl Pts',(-35.9240485500601,0.962061761883848,
305.587215089976));
#11699=CARTESIAN_POINT('Ctrl Pts',(-35.9303953447993,0.947630666368683,
305.588299131218));
#11700=CARTESIAN_POINT('Ctrl Pts',(-35.9415781457625,0.921499695257981,
305.590238643671));
#11701=CARTESIAN_POINT('Ctrl Pts',(-35.9464652518913,0.9098223853355,305.591097004448));
#11702=CARTESIAN_POINT('Ctrl Pts',(-35.9566272859836,0.884984548943407,
305.592904421192));
#11703=CARTESIAN_POINT('Ctrl Pts',(-35.9618780728703,0.871814998228795,
305.593852091933));
#11704=CARTESIAN_POINT('Ctrl Pts',(-35.9762990463627,0.834681128292523,
305.596496519875));
#11705=CARTESIAN_POINT('Ctrl Pts',(-35.9851992106731,0.810613170955293,
305.598178312866));
#11706=CARTESIAN_POINT('Ctrl Pts',(-36.0433604898388,0.645125094243305,
305.609554450537));
#11707=CARTESIAN_POINT('Ctrl Pts',(-36.0795280818733,0.499442076294542,
305.61865449061));
#11708=CARTESIAN_POINT('Ctrl Pts',(-36.1190741471813,0.235401644859499,
305.635020122626));
#11709=CARTESIAN_POINT('Ctrl Pts',(-36.1278170067582,0.118383906896199,
305.642229472726));
#11710=CARTESIAN_POINT('Ctrl Pts',(-36.1278767173156,0.00120860362354279,
305.649679341437));
#11711=CARTESIAN_POINT('Ctrl Pts',(-36.1278766586888,0.00131864288668422,
305.651410108095));
#11712=CARTESIAN_POINT('Ctrl Pts',(-36.1279213776981,-0.0791142741799706,
305.656783719909));
#11713=CARTESIAN_POINT('Ctrl Pts',(-36.1238701842287,-0.159550669184445,
305.662157331723));
#11714=CARTESIAN_POINT('Ctrl Pts',(-36.1157484705838,-0.239551032677529,
305.667530943537));
#11715=CARTESIAN_POINT('Ctrl Pts',(-36.1076245801917,-0.319572837528005,
305.672905995564));
#11716=CARTESIAN_POINT('Ctrl Pts',(-36.0954280477296,-0.399157927229441,
305.678281047591));
#11717=CARTESIAN_POINT('Ctrl Pts',(-36.079236009608,-0.477873110072393,
305.683656099617));
#11718=CARTESIAN_POINT('Ctrl Pts',(-36.0630218193141,-0.556695982403609,
305.689038505201));
#11719=CARTESIAN_POINT('Ctrl Pts',(-36.0428012976816,-0.63464612534666,
305.694420910785));
#11720=CARTESIAN_POINT('Ctrl Pts',(-36.0187024588884,-0.711301953905909,
305.699803316369));
#11721=CARTESIAN_POINT('Ctrl Pts',(-35.9945873950798,-0.788009392503775,
305.705189345763));
#11722=CARTESIAN_POINT('Ctrl Pts',(-35.9665889709448,-0.863420355153572,
305.710575375157));
#11723=CARTESIAN_POINT('Ctrl Pts',(-35.9348838261372,-0.937132255938665,
305.715961404551));
#11724=CARTESIAN_POINT('Ctrl Pts',(-35.9031124904097,-1.0109980452665,305.721358678373));
#11725=CARTESIAN_POINT('Ctrl Pts',(-35.8676191689213,-1.08315727524832,
305.726755952196));
#11726=CARTESIAN_POINT('Ctrl Pts',(-35.8286271023704,-1.15323089312922,
305.732153226018));
#11727=CARTESIAN_POINT('Ctrl Pts',(-35.7904076459934,-1.2219160339456,305.7374435553));
#11728=CARTESIAN_POINT('Ctrl Pts',(-35.7488271282622,-1.28859716976929,
305.742733884581));
#11729=CARTESIAN_POINT('Ctrl Pts',(-35.7041344894103,-1.35294677726268,
305.748024213863));
#11730=CARTESIAN_POINT('Ctrl Pts',(-35.6590907331093,-1.41780193266302,
305.753356105401));
#11731=CARTESIAN_POINT('Ctrl Pts',(-35.6107192482689,-1.48052804985976,
305.758687996939));
#11732=CARTESIAN_POINT('Ctrl Pts',(-35.559248273395,-1.54076339099012,305.764019888477));
#11733=CARTESIAN_POINT('Ctrl Pts',(-35.5078517500581,-1.60091160313684,
305.769344067561));
#11734=CARTESIAN_POINT('Ctrl Pts',(-35.4533649419751,-1.6585758405409,305.774668246645));
#11735=CARTESIAN_POINT('Ctrl Pts',(-35.3960588605108,-1.71342395168949,
305.779992425729));
#11736=CARTESIAN_POINT('Ctrl Pts',(-35.3388195537606,-1.76820815222248,
305.785310400924));
#11737=CARTESIAN_POINT('Ctrl Pts',(-35.2787678387905,-1.82018242492944,
305.79062837612));
#11738=CARTESIAN_POINT('Ctrl Pts',(-35.2162133962421,-1.86904945139643,
305.795946351316));
#11739=CARTESIAN_POINT('Ctrl Pts',(-35.1536988713225,-1.91788529453343,
305.801260932972));
#11740=CARTESIAN_POINT('Ctrl Pts',(-35.0886851571728,-1.96361753912731,
305.806575514628));
#11741=CARTESIAN_POINT('Ctrl Pts',(-35.021516102623,-2.0059881717957,305.811890096285));
#11742=CARTESIAN_POINT('Ctrl Pts',(-34.954368982389,-2.04834496816933,305.817202942444));
#11743=CARTESIAN_POINT('Ctrl Pts',(-34.8850683155989,-2.08734208247314,
305.822515788603));
#11744=CARTESIAN_POINT('Ctrl Pts',(-34.8139868734757,-2.12276484897125,
305.827828634762));
#11745=CARTESIAN_POINT('Ctrl Pts',(-34.7429064967397,-2.15818708454371,
305.833141401291));
#11746=CARTESIAN_POINT('Ctrl Pts',(-34.6700458179381,-2.19003487088063,
305.838454167819));
#11747=CARTESIAN_POINT('Ctrl Pts',(-34.5958008016666,-2.21814021461921,
305.843766934348));
#11748=CARTESIAN_POINT('Ctrl Pts',(-34.521481688898,-2.24627360747983,305.849085003016));
#11749=CARTESIAN_POINT('Ctrl Pts',(-34.4457759183066,-2.27065693028045,
305.854403071683));
#11750=CARTESIAN_POINT('Ctrl Pts',(-34.3690974088338,-2.29117117897341,
305.859721140351));
#11751=CARTESIAN_POINT('Ctrl Pts',(-34.2923821790316,-2.3116952516702,305.865041755772));
#11752=CARTESIAN_POINT('Ctrl Pts',(-34.2146937413942,-2.32834646070103,
305.870362371193));
#11753=CARTESIAN_POINT('Ctrl Pts',(-34.1364565640286,-2.34105692037555,
305.875682986613));
#11754=CARTESIAN_POINT('Ctrl Pts',(-34.0580766698169,-2.35379056591616,
305.881013307669));
#11755=CARTESIAN_POINT('Ctrl Pts',(-33.9791465028503,-2.3625690456559,305.886343628724));
#11756=CARTESIAN_POINT('Ctrl Pts',(-33.900095825025,-2.3673764058961,305.891673949779));
#11757=CARTESIAN_POINT('Ctrl Pts',(-33.8246509406918,-2.37196448467352,
305.896761135197));
#11758=CARTESIAN_POINT('Ctrl Pts',(-33.749096658507,-2.37293585714187,305.901848320614));
#11759=CARTESIAN_POINT('Ctrl Pts',(-33.6738031839495,-2.37032083221919,
305.906935506032));
#11760=CARTESIAN_POINT('Ctrl Pts',(-33.5948879495595,-2.36758001960665,
305.912267394777));
#11761=CARTESIAN_POINT('Ctrl Pts',(-33.5159602124537,-2.36088871336514,
305.917599283523));
#11762=CARTESIAN_POINT('Ctrl Pts',(-33.4374476763346,-2.35024286725224,
305.922931172269));
#11763=CARTESIAN_POINT('Ctrl Pts',(-33.359048705301,-2.33961241990854,305.928255348661));
#11764=CARTESIAN_POINT('Ctrl Pts',(-33.2810642032751,-2.32503885442818,
305.933579525054));
#11765=CARTESIAN_POINT('Ctrl Pts',(-33.2039201677124,-2.30657010493505,
305.938903701446));
#11766=CARTESIAN_POINT('Ctrl Pts',(-33.1268660202592,-2.28812287519991,
305.944221674117));
#11767=CARTESIAN_POINT('Ctrl Pts',(-33.0506508467579,-2.26578958936141,
305.949539646787));
#11768=CARTESIAN_POINT('Ctrl Pts',(-32.9756923053248,-2.2396695538457,305.954857619458));
#11769=CARTESIAN_POINT('Ctrl Pts',(-32.9007815954792,-2.21356618571358,
305.960172198691));
#11770=CARTESIAN_POINT('Ctrl Pts',(-32.8271263676736,-2.18368101780014,
305.965486777925));
#11771=CARTESIAN_POINT('Ctrl Pts',(-32.7551297436213,-2.1501633669693,305.970801357159));
#11772=CARTESIAN_POINT('Ctrl Pts',(-32.6831566289195,-2.11665666079334,
305.976114201001));
#11773=CARTESIAN_POINT('Ctrl Pts',(-32.6128414672458,-2.07952002472724,
305.981427044843));
#11774=CARTESIAN_POINT('Ctrl Pts',(-32.5445666044412,-2.03895056566143,
305.986739888686));
#11775=CARTESIAN_POINT('Ctrl Pts',(-32.4762927635464,-1.99838171382254,
305.992052653008));
#11776=CARTESIAN_POINT('Ctrl Pts',(-32.4100595631882,-1.95438038175849,
305.99736541733));
#11777=CARTESIAN_POINT('Ctrl Pts',(-32.346222675646,-1.90718845095239,306.002678181652));
#11778=CARTESIAN_POINT('Ctrl Pts',(-32.2823220765991,-1.85994942090588,
306.007996248304));
#11779=CARTESIAN_POINT('Ctrl Pts',(-32.2208229458303,-1.80951371035004,
306.013314314955));
#11780=CARTESIAN_POINT('Ctrl Pts',(-32.1620494969452,-1.75616482604265,
306.018632381606));
#11781=CARTESIAN_POINT('Ctrl Pts',(-32.1032479011064,-1.7027903926378,306.023952995112));
#11782=CARTESIAN_POINT('Ctrl Pts',(-32.0471749189374,-1.64650033876582,
306.029273608617));
#11783=CARTESIAN_POINT('Ctrl Pts',(-31.99411750502,-1.58761472438755,306.034594222122));
#11784=CARTESIAN_POINT('Ctrl Pts',(-31.9409633040926,-1.52862169123154,
306.039924541458));
#11785=CARTESIAN_POINT('Ctrl Pts',(-31.8908359604425,-1.46702400086003,
306.045254860794));
#11786=CARTESIAN_POINT('Ctrl Pts',(-31.8439816394093,-1.40317428920256,
306.050585180129));
#11787=CARTESIAN_POINT('Ctrl Pts',(-31.7992643215169,-1.34223673231215,
306.055672386153));
#11788=CARTESIAN_POINT('Ctrl Pts',(-31.7575281364002,-1.27924842454727,
306.060759592177));
#11789=CARTESIAN_POINT('Ctrl Pts',(-31.7189481061582,-1.21453699576303,
306.065846798201));
#11790=CARTESIAN_POINT('Ctrl Pts',(-31.6785125504094,-1.14671323902197,
306.071178675898));
#11791=CARTESIAN_POINT('Ctrl Pts',(-31.6413911575609,-1.07673942831649,
306.076510553594));
#11792=CARTESIAN_POINT('Ctrl Pts',(-31.6078189698145,-1.00497291576352,
306.081842431291));
#11793=CARTESIAN_POINT('Ctrl Pts',(-31.5742953443195,-0.933310213645913,
306.087166596414));
#11794=CARTESIAN_POINT('Ctrl Pts',(-31.5443109256388,-0.859860380399543,
306.092490761536));
#11795=CARTESIAN_POINT('Ctrl Pts',(-31.5180561351155,-0.785007486077892,
306.097814926659));
#11796=CARTESIAN_POINT('Ctrl Pts',(-31.4918319380809,-0.710241814359655,
306.103132887779));
#11797=CARTESIAN_POINT('Ctrl Pts',(-31.4693288871985,-0.634076770637978,
306.108450848899));
#11798=CARTESIAN_POINT('Ctrl Pts',(-31.4506897016496,-0.556917237491704,
306.113768810019));
#11799=CARTESIAN_POINT('Ctrl Pts',(-31.4320624105057,-0.479806942909443,
306.119083377537));
#11800=CARTESIAN_POINT('Ctrl Pts',(-31.4172942005321,-0.401703873022735,
306.124397945055));
#11801=CARTESIAN_POINT('Ctrl Pts',(-31.4064778772932,-0.323027775849396,
306.129712512573));
#11802=CARTESIAN_POINT('Ctrl Pts',(-31.3956650862638,-0.244377371367967,
306.13502534455));
#11803=CARTESIAN_POINT('Ctrl Pts',(-31.3888016831451,-0.165154775304011,
306.140338176528));
#11804=CARTESIAN_POINT('Ctrl Pts',(-31.3859290471889,-0.085788153373663,
306.145651008505));
#11805=CARTESIAN_POINT('Ctrl Pts',(-31.3830564543013,-0.00642272136167781,
306.150963760829));
#11806=CARTESIAN_POINT('Ctrl Pts',(-31.3841745252713,0.073086263643561,
306.156276513153));
#11807=CARTESIAN_POINT('Ctrl Pts',(-31.3892725537851,0.15230880923493,306.161589265477));
#11808=CARTESIAN_POINT('Ctrl Pts',(-31.3943756702046,0.231610420064857,
306.166907320004));
#11809=CARTESIAN_POINT('Ctrl Pts',(-31.4034666487077,0.310624551427704,
306.172225374531));
#11810=CARTESIAN_POINT('Ctrl Pts',(-31.4164827532814,0.38892511246911,306.177543429058));
#11811=CARTESIAN_POINT('Ctrl Pts',(-31.429505091142,0.467263170893507,306.18286403035));
#11812=CARTESIAN_POINT('Ctrl Pts',(-31.4464561995775,0.544886519556357,
306.188184631642));
#11813=CARTESIAN_POINT('Ctrl Pts',(-31.4672224352513,0.621380592188205,
306.193505232934));
#11814=CARTESIAN_POINT('Ctrl Pts',(-31.4880265526266,0.698014205065533,
306.19883554005));
#11815=CARTESIAN_POINT('Ctrl Pts',(-31.5126595583196,0.773513978588081,
306.204165847166));
#11816=CARTESIAN_POINT('Ctrl Pts',(-31.5409583331658,0.847481992773977,
306.209496154282));
#11817=CARTESIAN_POINT('Ctrl Pts',(-31.5679670391485,0.91807799412496,306.214583466311));
#11818=CARTESIAN_POINT('Ctrl Pts',(-31.5983143888503,0.987278539532674,
306.219670778341));
#11819=CARTESIAN_POINT('Ctrl Pts',(-31.6318197407079,1.0547590356613,306.22475809037));
#11820=CARTESIAN_POINT('Ctrl Pts',(-31.6669302309801,1.12547231492948,306.230089119881));
#11821=CARTESIAN_POINT('Ctrl Pts',(-31.70564191788,1.19456452682633,306.235420149392));
#11822=CARTESIAN_POINT('Ctrl Pts',(-31.7477817782138,1.26164473255218,306.240751178903));
#11823=CARTESIAN_POINT('Ctrl Pts',(-31.7898643495412,1.32863374295119,306.246074960896));
#11824=CARTESIAN_POINT('Ctrl Pts',(-31.8353655959063,1.39361578338627,306.251398742889));
#11825=CARTESIAN_POINT('Ctrl Pts',(-31.8840658378854,1.45622284463428,306.256722524882));
#11826=CARTESIAN_POINT('Ctrl Pts',(-31.9327150532832,1.51876430817316,306.262040728784));
#11827=CARTESIAN_POINT('Ctrl Pts',(-31.9845563219832,1.57893536591941,306.267358932686));
#11828=CARTESIAN_POINT('Ctrl Pts',(-32.0393265503279,1.63639670978073,306.272677136587));
#11829=CARTESIAN_POINT('Ctrl Pts',(-32.094058522837,1.69381791811966,306.277991625837));
#11830=CARTESIAN_POINT('Ctrl Pts',(-32.1517150689476,1.74853283334435,306.283306115087));
#11831=CARTESIAN_POINT('Ctrl Pts',(-32.2119936138942,1.80023611518357,306.288620604337));
#11832=CARTESIAN_POINT('Ctrl Pts',(-32.2722481476732,1.85191880169874,306.29393297663));
#11833=CARTESIAN_POINT('Ctrl Pts',(-32.3351222478881,1.90059193545501,306.299245348923));
#11834=CARTESIAN_POINT('Ctrl Pts',(-32.4002784866108,1.94598890098306,306.304557721215));
#11835=CARTESIAN_POINT('Ctrl Pts',(-32.4654418309203,1.99139081725853,306.309870672847));
#11836=CARTESIAN_POINT('Ctrl Pts',(-32.5328874271204,2.03351558229234,306.315183624478));
#11837=CARTESIAN_POINT('Ctrl Pts',(-32.6022479731971,2.07213927999928,306.32049657611));
#11838=CARTESIAN_POINT('Ctrl Pts',(-32.624620279292,2.08459738819613,306.322210273404));
#11839=CARTESIAN_POINT('Ctrl Pts',(-32.6471916083291,2.09669159721057,306.323923970699));
#11840=CARTESIAN_POINT('Ctrl Pts',(-32.6699490794746,2.10841540797695,306.325637667993));
#11841=CARTESIAN_POINT('Origin',(-33.7561270252576,0.,302.151410108095));
#11842=CARTESIAN_POINT('',(-32.669948905789,2.10841531850051,307.52304986714));
#11843=CARTESIAN_POINT('',(-32.6683119391961,2.11155019427352,307.325629814339));
#11844=CARTESIAN_POINT('',(-32.6699490794746,2.10841540797695,302.151410108095));
#11845=CARTESIAN_POINT('',(-36.127877017276,-0.000194578459783513,306.846254750936));
#11846=CARTESIAN_POINT('Ctrl Pts',(-32.669948905789,2.10841531850051,307.52304986714));
#11847=CARTESIAN_POINT('Ctrl Pts',(-32.6291536046931,2.08739907799101,307.519703664692));
#11848=CARTESIAN_POINT('Ctrl Pts',(-32.5889626779185,2.06519595461221,307.516347061658));
#11849=CARTESIAN_POINT('Ctrl Pts',(-32.463472090138,1.99103245979216,307.505708193501));
#11850=CARTESIAN_POINT('Ctrl Pts',(-32.3808016729988,1.93485161061858,307.498456265159));
#11851=CARTESIAN_POINT('Ctrl Pts',(-32.2809745266202,1.85737063800947,307.489581439048));
#11852=CARTESIAN_POINT('Ctrl Pts',(-32.2603089829766,1.84076861973144,307.48773765135));
#11853=CARTESIAN_POINT('Ctrl Pts',(-32.2287706654417,1.8145498124291,307.484918969574));
#11854=CARTESIAN_POINT('Ctrl Pts',(-32.2177012029804,1.80517436519654,307.483928713116));
#11855=CARTESIAN_POINT('Ctrl Pts',(-32.1971102178872,1.78740753440575,307.482086024239));
#11856=CARTESIAN_POINT('Ctrl Pts',(-32.1875694449029,1.77904081578627,307.48123208744));
#11857=CARTESIAN_POINT('Ctrl Pts',(-32.1645217353442,1.75849972073287,307.479167942608));
#11858=CARTESIAN_POINT('Ctrl Pts',(-32.1510868622955,1.74624591422736,307.477963533858));
#11859=CARTESIAN_POINT('Ctrl Pts',(-32.1010312430896,1.69952490619419,307.473465557447));
#11860=CARTESIAN_POINT('Ctrl Pts',(-32.0653663687863,1.66404812675948,307.470238901108));
#11861=CARTESIAN_POINT('Ctrl Pts',(-31.9686412486793,1.56150974645989,307.461330643034));
#11862=CARTESIAN_POINT('Ctrl Pts',(-31.9102574576355,1.4920407832551,307.455763108366));
#11863=CARTESIAN_POINT('Ctrl Pts',(-31.7618294183545,1.29334116534389,307.440559666581));
#11864=CARTESIAN_POINT('Ctrl Pts',(-31.6804534809308,1.15824326746686,307.430955875689));
#11865=CARTESIAN_POINT('Ctrl Pts',(-31.5959157346897,0.979941685904312,
307.418300152065));
#11866=CARTESIAN_POINT('Ctrl Pts',(-31.579694916916,0.94336710970338,307.415707152027));
#11867=CARTESIAN_POINT('Ctrl Pts',(-31.5551614972478,0.88404419762547,307.411495744531));
#11868=CARTESIAN_POINT('Ctrl Pts',(-31.5462584197052,0.86154748692908,307.409897441728));
#11869=CARTESIAN_POINT('Ctrl Pts',(-31.5297912858489,0.818002037920552,
307.406799257714));
#11870=CARTESIAN_POINT('Ctrl Pts',(-31.5221777350071,0.796974697133103,
307.405301236171));
#11871=CARTESIAN_POINT('Ctrl Pts',(-31.505001215033,0.747354998155642,307.401760133146));
#11872=CARTESIAN_POINT('Ctrl Pts',(-31.4956840415227,0.718682320381088,
307.399709175678));
#11873=CARTESIAN_POINT('Ctrl Pts',(-31.4648482700424,0.617248992593758,
307.392433501489));
#11874=CARTESIAN_POINT('Ctrl Pts',(-31.4462785702959,0.54364750578791,307.387116218976));
#11875=CARTESIAN_POINT('Ctrl Pts',(-31.4050818909819,0.33955925022164,307.372275708274));
#11876=CARTESIAN_POINT('Ctrl Pts',(-31.3898014674528,0.207873854870359,
307.36258171725));
#11877=CARTESIAN_POINT('Ctrl Pts',(-31.3822919101746,-0.0275512204801254,
307.34540000574));
#11878=CARTESIAN_POINT('Ctrl Pts',(-31.3857390502401,-0.13083361538035,
307.337919144375));
#11879=CARTESIAN_POINT('Ctrl Pts',(-31.3980717522607,-0.255454347045799,
307.329180950194));
#11880=CARTESIAN_POINT('Ctrl Pts',(-31.4005415966385,-0.277306635222439,
307.327659755259));
#11881=CARTESIAN_POINT('Ctrl Pts',(-31.4050062455816,-0.312424299571121,
307.325236244969));
#11882=CARTESIAN_POINT('Ctrl Pts',(-31.4068102012905,-0.32571206095583,
307.32432412947));
#11883=CARTESIAN_POINT('Ctrl Pts',(-31.4106274339495,-0.352145659643509,
307.32252034031));
#11884=CARTESIAN_POINT('Ctrl Pts',(-31.4126387662875,-0.365291251296927,
307.321628610258));
#11885=CARTESIAN_POINT('Ctrl Pts',(-31.4181852859462,-0.399608804941246,
307.319312920007));
#11886=CARTESIAN_POINT('Ctrl Pts',(-31.4218975913983,-0.420751475337849,
307.317898458906));
#11887=CARTESIAN_POINT('Ctrl Pts',(-31.4428452991858,-0.53122765141641,
307.310557736726));
#11888=CARTESIAN_POINT('Ctrl Pts',(-31.4649251696897,-0.61957480390495,
307.304858643912));
#11889=CARTESIAN_POINT('Ctrl Pts',(-31.5532868691836,-0.902767303017338,
307.286523586627));
#11890=CARTESIAN_POINT('Ctrl Pts',(-31.6398114074909,-1.09027448089469,
307.274194698425));
#11891=CARTESIAN_POINT('Ctrl Pts',(-31.7693483967489,-1.29587977526629,
307.2585658805));
#11892=CARTESIAN_POINT('Ctrl Pts',(-31.7900055127924,-1.32701155225187,
307.25613904528));
#11893=CARTESIAN_POINT('Ctrl Pts',(-31.8249358002462,-1.37704707161445,
307.252130037151));
#11894=CARTESIAN_POINT('Ctrl Pts',(-31.8387725274328,-1.39624849015093,
307.250564474461));
#11895=CARTESIAN_POINT('Ctrl Pts',(-31.8663784218923,-1.4333732806422,307.247482109363));
#11896=CARTESIAN_POINT('Ctrl Pts',(-31.8801210435141,-1.45131328138309,
307.245966455723));
#11897=CARTESIAN_POINT('Ctrl Pts',(-31.9137231717789,-1.49390361330038,
307.242303216889));
#11898=CARTESIAN_POINT('Ctrl Pts',(-31.93382345473,-1.51835749833102,307.240146147827));
#11899=CARTESIAN_POINT('Ctrl Pts',(-32.0123060027435,-1.61003511820792,
307.231846787389));
#11900=CARTESIAN_POINT('Ctrl Pts',(-32.0739611617507,-1.67434747359036,
307.225572526693));
#11901=CARTESIAN_POINT('Ctrl Pts',(-32.2835017710116,-1.8696386891287,307.205021418415));
#11902=CARTESIAN_POINT('Ctrl Pts',(-32.4441533212775,-1.98567190297956,
307.190315173605));
#11903=CARTESIAN_POINT('Ctrl Pts',(-32.6480129420326,-2.09726151902507,
307.173852996177));
#11904=CARTESIAN_POINT('Ctrl Pts',(-32.6790799459142,-2.11338415854509,
307.17140125084));
#11905=CARTESIAN_POINT('Ctrl Pts',(-32.7248046178473,-2.13584324003085,
307.167886455046));
#11906=CARTESIAN_POINT('Ctrl Pts',(-32.7391859621059,-2.14272797248362,
307.166794199414));
#11907=CARTESIAN_POINT('Ctrl Pts',(-32.7649688993926,-2.15475288603087,
307.164860893863));
#11908=CARTESIAN_POINT('Ctrl Pts',(-32.7763430621495,-2.15994857207763,
307.164016672615));
#11909=CARTESIAN_POINT('Ctrl Pts',(-32.8024597365458,-2.17162983084127,
307.162097771747));
#11910=CARTESIAN_POINT('Ctrl Pts',(-32.8172279211728,-2.17805553846788,
307.161026627419));
#11911=CARTESIAN_POINT('Ctrl Pts',(-32.8651627584999,-2.19833404354466,
307.157591101519));
#11912=CARTESIAN_POINT('Ctrl Pts',(-32.898580766007,-2.21158419117673,307.155259228338));
#11913=CARTESIAN_POINT('Ctrl Pts',(-32.9824506994427,-2.24265120677377,
307.149531937816));
#11914=CARTESIAN_POINT('Ctrl Pts',(-33.0332296848043,-2.25953084197437,
307.146174555644));
#11915=CARTESIAN_POINT('Ctrl Pts',(-33.1776413132687,-2.30216767044983,
307.136822321827));
#11916=CARTESIAN_POINT('Ctrl Pts',(-33.2723458175848,-2.32391447656752,
307.130913013371));
#11917=CARTESIAN_POINT('Ctrl Pts',(-33.4941140570786,-2.36069028902384,
307.117108850802));
#11918=CARTESIAN_POINT('Ctrl Pts',(-33.6215764974871,-2.371370927097,307.109191088827));
#11919=CARTESIAN_POINT('Ctrl Pts',(-33.7838572571033,-2.37184007913191,
307.098721271738));
#11920=CARTESIAN_POINT('Ctrl Pts',(-33.8184406679319,-2.37118348851954,
307.096468703635));
#11921=CARTESIAN_POINT('Ctrl Pts',(-33.8737970864208,-2.36892068858804,
307.092822555602));
#11922=CARTESIAN_POINT('Ctrl Pts',(-33.8945855277575,-2.36779658511583,
307.091444131109));
#11923=CARTESIAN_POINT('Ctrl Pts',(-33.937916761463,-2.36488093778276,307.088550453095));
#11924=CARTESIAN_POINT('Ctrl Pts',(-33.9604540225239,-2.36304036673669,
307.087033797287));
#11925=CARTESIAN_POINT('Ctrl Pts',(-34.0145491136094,-2.35784289459128,
307.083363943893));
#11926=CARTESIAN_POINT('Ctrl Pts',(-34.0460718556148,-2.35417435975609,
307.081201174547));
#11927=CARTESIAN_POINT('Ctrl Pts',(-34.1665114209254,-2.33770230992993,
307.072840528105));
#11928=CARTESIAN_POINT('Ctrl Pts',(-34.254738461866,-2.32048499372037,307.066508068907));
#11929=CARTESIAN_POINT('Ctrl Pts',(-34.5393270065787,-2.24796789465653,
307.045429536507));
#11930=CARTESIAN_POINT('Ctrl Pts',(-34.7295558522013,-2.17237028144524,
307.030220244785));
#11931=CARTESIAN_POINT('Ctrl Pts',(-34.9341073994896,-2.05875400215761,
307.013725392309));
#11932=CARTESIAN_POINT('Ctrl Pts',(-34.9601663288664,-2.04362309802117,
307.011623146056));
#11933=CARTESIAN_POINT('Ctrl Pts',(-34.9988112104367,-2.02018835145821,
307.008512000459));
#11934=CARTESIAN_POINT('Ctrl Pts',(-35.0116168706243,-2.01225501326667,
307.007482158663));
#11935=CARTESIAN_POINT('Ctrl Pts',(-35.0349676077063,-1.99747911242623,
307.005607520721));
#11936=CARTESIAN_POINT('Ctrl Pts',(-35.0455346995024,-1.99067423254084,
307.004760553942));
#11937=CARTESIAN_POINT('Ctrl Pts',(-35.0704385735836,-1.97435539521378,
307.002767124403));
#11938=CARTESIAN_POINT('Ctrl Pts',(-35.0847266784049,-1.9647689630405,307.001625399393));
#11939=CARTESIAN_POINT('Ctrl Pts',(-35.1343392524853,-1.93069327637295,
306.997663130212));
#11940=CARTESIAN_POINT('Ctrl Pts',(-35.1691033488349,-1.9053986232599,306.99489053457));
#11941=CARTESIAN_POINT('Ctrl Pts',(-35.2586541431049,-1.83644097495435,
306.987703199578));
#11942=CARTESIAN_POINT('Ctrl Pts',(-35.3122289333961,-1.79127086295319,
306.983356113053));
#11943=CARTESIAN_POINT('Ctrl Pts',(-35.5017791844257,-1.61652458723488,
306.967479284102));
#11944=CARTESIAN_POINT('Ctrl Pts',(-35.624216946341,-1.47332560575195,306.956156254573));
#11945=CARTESIAN_POINT('Ctrl Pts',(-35.7506777173988,-1.28396343557345,
306.941551397319));
#11946=CARTESIAN_POINT('Ctrl Pts',(-35.7720237750796,-1.25018181106343,
306.938961502858));
#11947=CARTESIAN_POINT('Ctrl Pts',(-35.8049033167822,-1.19511448344296,
306.934753883871));
#11948=CARTESIAN_POINT('Ctrl Pts',(-35.8169824648313,-1.17416255506173,
306.933156196315));
#11949=CARTESIAN_POINT('Ctrl Pts',(-35.8396121876671,-1.13348484492079,
306.930058373272));
#11950=CARTESIAN_POINT('Ctrl Pts',(-35.8502082629263,-1.11378724464323,
306.928560084849));
#11951=CARTESIAN_POINT('Ctrl Pts',(-35.8744401003821,-1.06717294373351,
306.925017024253));
#11952=CARTESIAN_POINT('Ctrl Pts',(-35.8878436423616,-1.04014061246904,
306.922964350476));
#11953=CARTESIAN_POINT('Ctrl Pts',(-35.9332106445632,-0.944081936041073,
306.915673591037));
#11954=CARTESIAN_POINT('Ctrl Pts',(-35.9623630611649,-0.873787255719231,
306.910342415322));
#11955=CARTESIAN_POINT('Ctrl Pts',(-36.0260686944148,-0.696543641088698,
306.89691609023));
#11956=CARTESIAN_POINT('Ctrl Pts',(-36.056495417909,-0.588310919215101,
306.888725877847));
#11957=CARTESIAN_POINT('Ctrl Pts',(-36.1019991305066,-0.367326364621391,
306.872245732569));
#11958=CARTESIAN_POINT('Ctrl Pts',(-36.116873116569,-0.254807449769235,
306.863977309298));
#11959=CARTESIAN_POINT('Ctrl Pts',(-36.125250290397,-0.114790745098507,
306.854119245306));
#11960=CARTESIAN_POINT('Ctrl Pts',(-36.1264001201571,-0.0879065852303928,
306.852246352496));
#11961=CARTESIAN_POINT('Ctrl Pts',(-36.1274096809125,-0.048671399532048,
306.849547474942));
#11962=CARTESIAN_POINT('Ctrl Pts',(-36.1276308264995,-0.0363328465487193,
306.848703708325));
#11963=CARTESIAN_POINT('Ctrl Pts',(-36.1278359145932,-0.0160603911082621,
306.847326153347));
#11964=CARTESIAN_POINT('Ctrl Pts',(-36.1278763664462,-0.00812765307939112,
306.846789323244));
#11965=CARTESIAN_POINT('Ctrl Pts',(-36.127877017276,-0.000194578459783513,
306.846254750936));
#11966=CARTESIAN_POINT('Ctrl Pts',(-36.1278770172634,-0.000194731713651253,
306.846254761263));
#11967=CARTESIAN_POINT('Ctrl Pts',(-36.1278774563459,0.00515310811414783,
306.845894395659));
#11968=CARTESIAN_POINT('Ctrl Pts',(-36.1278598079454,0.0105009685530968,
306.845535050245));
#11969=CARTESIAN_POINT('Ctrl Pts',(-36.1277582570605,0.0256975957702179,
306.844516710825));
#11970=CARTESIAN_POINT('Ctrl Pts',(-36.1276310938811,0.0355461262819293,
306.843860077856));
#11971=CARTESIAN_POINT('Ctrl Pts',(-36.1270154865911,0.0677046885558121,
306.841725987912));
#11972=CARTESIAN_POINT('Ctrl Pts',(-36.1262735210064,0.0900094268948125,
306.840261568538));
#11973=CARTESIAN_POINT('Ctrl Pts',(-36.1197048925516,0.228580092810293,
306.831243183719));
#11974=CARTESIAN_POINT('Ctrl Pts',(-36.1056389628918,0.344310022035404,
306.824054824637));
#11975=CARTESIAN_POINT('Ctrl Pts',(-36.0608152101483,0.571776512456467,
306.809824522904));
#11976=CARTESIAN_POINT('Ctrl Pts',(-36.0302701490589,0.683218723248633,
306.80279845525));
#11977=CARTESIAN_POINT('Ctrl Pts',(-35.9664306693679,0.863422495560842,
306.790851462533));
#11978=CARTESIAN_POINT('Ctrl Pts',(-35.9377191958462,0.933592260668311,
306.786045212838));
#11979=CARTESIAN_POINT('Ctrl Pts',(-35.8929660106762,1.02957532602775,306.779172980922));
#11980=CARTESIAN_POINT('Ctrl Pts',(-35.8797124208884,1.05664144027858,306.777200909041));
#11981=CARTESIAN_POINT('Ctrl Pts',(-35.85573235748,1.10333835807569,306.773734181727));
#11982=CARTESIAN_POINT('Ctrl Pts',(-35.8452370004536,1.12308394012621,306.772247771746));
#11983=CARTESIAN_POINT('Ctrl Pts',(-35.8228058219585,1.16388245970358,306.769131903066));
#11984=CARTESIAN_POINT('Ctrl Pts',(-35.8108238718769,1.1849069252816,306.7675009167));
#11985=CARTESIAN_POINT('Ctrl Pts',(-35.778172505885,1.24021470579082,306.763140767886));
#11986=CARTESIAN_POINT('Ctrl Pts',(-35.7569540314417,1.27416301722768,306.760391945756));
#11987=CARTESIAN_POINT('Ctrl Pts',(-35.6314170739579,1.46414151122691,306.744581501467));
#11988=CARTESIAN_POINT('Ctrl Pts',(-35.5097406367729,1.60786764857421,306.730863155621));
#11989=CARTESIAN_POINT('Ctrl Pts',(-35.3028887619339,1.80048792503961,306.710246681824));
#11990=CARTESIAN_POINT('Ctrl Pts',(-35.2295071613655,1.86101662323564,306.703357205578));
#11991=CARTESIAN_POINT('Ctrl Pts',(-35.1314645679029,1.93244250150146,306.69484399385));
#11992=CARTESIAN_POINT('Ctrl Pts',(-35.1099875779095,1.94754951784499,306.693018863923));
#11993=CARTESIAN_POINT('Ctrl Pts',(-35.0764317457653,1.97032941381941,306.690233300838));
#11994=CARTESIAN_POINT('Ctrl Pts',(-35.0645276289194,1.97825439238528,306.689257645768));
#11995=CARTESIAN_POINT('Ctrl Pts',(-35.0418689585642,1.99304503340415,306.687425230021));
#11996=CARTESIAN_POINT('Ctrl Pts',(-35.0311296775771,1.99993226582504,306.68656718667));
#11997=CARTESIAN_POINT('Ctrl Pts',(-35.0071002039374,2.01507043276041,306.684669437456));
#11998=CARTESIAN_POINT('Ctrl Pts',(-34.9937827194217,2.02327733099054,306.683632505095));
#11999=CARTESIAN_POINT('Ctrl Pts',(-34.9461625215303,2.05197712434194,306.679973410174));
#12000=CARTESIAN_POINT('Ctrl Pts',(-34.9114223774695,2.07173542798703,306.677392893843));
#12001=CARTESIAN_POINT('Ctrl Pts',(-34.7086783487885,2.18035817473198,306.662739506664));
#12002=CARTESIAN_POINT('Ctrl Pts',(-34.530967085463,2.24965602621045,306.651420652043));
#12003=CARTESIAN_POINT('Ctrl Pts',(-34.2616230269383,2.31892659538957,306.634142759693));
#12004=CARTESIAN_POINT('Ctrl Pts',(-34.1752242892763,2.33608685157348,306.628591982323));
#12005=CARTESIAN_POINT('Ctrl Pts',(-34.0568391114912,2.35282078874392,306.62084867567));
#12006=CARTESIAN_POINT('Ctrl Pts',(-34.0255166080271,2.35661250970322,306.618787454681));
#12007=CARTESIAN_POINT('Ctrl Pts',(-33.9716618704988,2.36204417782628,306.615217182898));
#12008=CARTESIAN_POINT('Ctrl Pts',(-33.949164249989,2.36398911531894,306.613717897667));
#12009=CARTESIAN_POINT('Ctrl Pts',(-33.9030059654058,2.36731625444962,306.610624166743));
#12010=CARTESIAN_POINT('Ctrl Pts',(-33.8793455685378,2.36866561406213,306.609028863294));
#12011=CARTESIAN_POINT('Ctrl Pts',(-33.8181857857007,2.37123476112112,306.604878922486));
#12012=CARTESIAN_POINT('Ctrl Pts',(-33.7806718254818,2.37191965606312,306.602307923069));
#12013=CARTESIAN_POINT('Ctrl Pts',(-33.5382358164977,2.37059408799022,306.585518638005));
#12014=CARTESIAN_POINT('Ctrl Pts',(-33.3343521135606,2.3429185690601,306.570485717552));
#12015=CARTESIAN_POINT('Ctrl Pts',(-33.0484023640538,2.2655407613773,306.548919674832));
#12016=CARTESIAN_POINT('Ctrl Pts',(-32.9616345153684,2.23658986085814,306.542326023611));
#12017=CARTESIAN_POINT('Ctrl Pts',(-32.856794722381,2.19473483371029,306.5344552064));
#12018=CARTESIAN_POINT('Ctrl Pts',(-32.8369512080468,2.18649845195985,306.532970010008));
#12019=CARTESIAN_POINT('Ctrl Pts',(-32.8050063192341,2.17272741137367,306.530589592997));
#12020=CARTESIAN_POINT('Ctrl Pts',(-32.7928352520656,2.1673587578273,306.529685153995));
#12021=CARTESIAN_POINT('Ctrl Pts',(-32.7684909059324,2.15637488552004,306.527882095618));
#12022=CARTESIAN_POINT('Ctrl Pts',(-32.7563187983768,2.15075830414283,306.526983595275));
#12023=CARTESIAN_POINT('Ctrl Pts',(-32.7243250686593,2.13566510624946,306.52462823978));
#12024=CARTESIAN_POINT('Ctrl Pts',(-32.7045858611095,2.12601551960761,306.52318149419));
#12025=CARTESIAN_POINT('Ctrl Pts',(-32.6799621861859,2.1135512688101,306.521381323964));
#12026=CARTESIAN_POINT('Ctrl Pts',(-32.6749509397694,2.1109921821394,306.521015205799));
#12027=CARTESIAN_POINT('Ctrl Pts',(-32.669949078383,2.10841540741463,306.520649966606));
#12028=CARTESIAN_POINT('',(-36.12787621691,-0.00195816148385779,306.651410108095));
#12029=CARTESIAN_POINT('Ctrl Pts',(-32.6699490794746,2.10841540797695,306.325637667993));
#12030=CARTESIAN_POINT('Ctrl Pts',(-32.740580335012,2.14480202882853,306.330956386877));
#12031=CARTESIAN_POINT('Ctrl Pts',(-32.8130060340432,2.17761708796589,306.336275105761));
#12032=CARTESIAN_POINT('Ctrl Pts',(-32.8868275626125,2.20669810049877,306.341593824645));
#12033=CARTESIAN_POINT('Ctrl Pts',(-32.9606910905097,2.23579565811012,306.346915569511));
#12034=CARTESIAN_POINT('Ctrl Pts',(-33.0359515845324,2.26115479003096,306.352237314377));
#12035=CARTESIAN_POINT('Ctrl Pts',(-33.1121945935353,2.28266271837875,306.357559059243));
#12036=CARTESIAN_POINT('Ctrl Pts',(-33.1885688716104,2.30420767734527,306.36288996666));
#12037=CARTESIAN_POINT('Ctrl Pts',(-33.2659285853022,2.32188808823443,306.368220874078));
#12038=CARTESIAN_POINT('Ctrl Pts',(-33.3438488339219,2.33564225759189,306.373551781495));
#12039=CARTESIAN_POINT('Ctrl Pts',(-33.3931441306437,2.34434366539857,306.376924315177));
#12040=CARTESIAN_POINT('Ctrl Pts',(-33.4426636274186,2.35147471381064,306.380296848858));
#12041=CARTESIAN_POINT('Ctrl Pts',(-33.4922993170496,2.35703054771926,306.38366938254));
#12042=CARTESIAN_POINT('Ctrl Pts',(-33.5707719805349,2.36581416869707,306.38900126576));
#12043=CARTESIAN_POINT('Ctrl Pts',(-33.6498324657182,2.37069126356453,306.394333148981));
#12044=CARTESIAN_POINT('Ctrl Pts',(-33.7290582212338,2.37159552671798,306.399665032201));
#12045=CARTESIAN_POINT('Ctrl Pts',(-33.8081693780082,2.37249848186977,306.404989202941));
#12046=CARTESIAN_POINT('Ctrl Pts',(-33.8874448655169,2.36944001201456,306.410313373681));
#12047=CARTESIAN_POINT('Ctrl Pts',(-33.9664562485564,2.36240548600924,306.415637544421));
#12048=CARTESIAN_POINT('Ctrl Pts',(-34.0453755650935,2.35537915685075,306.420955511273));
#12049=CARTESIAN_POINT('Ctrl Pts',(-34.1240309241399,2.34438601973636,306.426273478125));
#12050=CARTESIAN_POINT('Ctrl Pts',(-34.2019946575969,2.32946348263547,306.431591444977));
#12051=CARTESIAN_POINT('Ctrl Pts',(-34.2799086403339,2.31455046800011,306.436906018293));
#12052=CARTESIAN_POINT('Ctrl Pts',(-34.3571314142341,2.29571311813722,306.44222059161));
#12053=CARTESIAN_POINT('Ctrl Pts',(-34.4332424076483,2.2730404355026,306.447535164926));
#12054=CARTESIAN_POINT('Ctrl Pts',(-34.5093285469098,2.25037515666464,306.452848002761));
#12055=CARTESIAN_POINT('Ctrl Pts',(-34.5843031776156,2.22387716576713,306.458160840596));
#12056=CARTESIAN_POINT('Ctrl Pts',(-34.6577593209395,2.19368577191067,306.463473678431));
#12057=CARTESIAN_POINT('Ctrl Pts',(-34.7312143636644,2.16349483041418,306.468786436664));
#12058=CARTESIAN_POINT('Ctrl Pts',(-34.8031505310992,2.12961077542176,306.474099194896));
#12059=CARTESIAN_POINT('Ctrl Pts',(-34.8731807112876,2.09222109850439,306.479411953129));
#12060=CARTESIAN_POINT('Ctrl Pts',(-34.9432807830373,2.0547941059198,306.484730013603));
#12061=CARTESIAN_POINT('Ctrl Pts',(-35.0114706530401,2.0138547236573,306.490048074078));
#12062=CARTESIAN_POINT('Ctrl Pts',(-35.0773882690518,1.96963620705639,306.495366134552));
#12063=CARTESIAN_POINT('Ctrl Pts',(-35.1433374527221,1.9253965144008,306.500686741823));
#12064=CARTESIAN_POINT('Ctrl Pts',(-35.2070118383397,1.87787483980058,306.506007349093));
#12065=CARTESIAN_POINT('Ctrl Pts',(-35.2680809106938,1.82734602930435,306.511327956364));
#12066=CARTESIAN_POINT('Ctrl Pts',(-35.3292613847221,1.77672504458852,306.51665826944));
#12067=CARTESIAN_POINT('Ctrl Pts',(-35.3878267019854,1.72308627990384,306.521988582516));
#12068=CARTESIAN_POINT('Ctrl Pts',(-35.4434819562292,1.66674275142438,306.527318895592));
#12069=CARTESIAN_POINT('Ctrl Pts',(-35.496599423864,1.61296839370921,306.532406155298));
#12070=CARTESIAN_POINT('Ctrl Pts',(-35.5470662239413,1.5567308559791,306.537493415003));
#12071=CARTESIAN_POINT('Ctrl Pts',(-35.5946614695316,1.49832878892391,306.542580674709));
#12072=CARTESIAN_POINT('Ctrl Pts',(-35.6443558396156,1.43735097700345,306.547892301183));
#12073=CARTESIAN_POINT('Ctrl Pts',(-35.6911130175382,1.37377573384131,306.553203927657));
#12074=CARTESIAN_POINT('Ctrl Pts',(-35.734648440398,1.30791860309843,306.558515554131));
#12075=CARTESIAN_POINT('Ctrl Pts',(-35.7781234778771,1.24215281884183,306.563819813166));
#12076=CARTESIAN_POINT('Ctrl Pts',(-35.8183853700947,1.17411181772676,306.569124072201));
#12077=CARTESIAN_POINT('Ctrl Pts',(-35.8551894739287,1.10414441948464,306.574428331236));
#12078=CARTESIAN_POINT('Ctrl Pts',(-35.891954203411,1.03425187487723,306.579726915584));
#12079=CARTESIAN_POINT('Ctrl Pts',(-35.9252682694939,0.962437439897806,
306.585025499932));
#12080=CARTESIAN_POINT('Ctrl Pts',(-35.954930930203,0.889077865036043,306.59032408428));
#12081=CARTESIAN_POINT('Ctrl Pts',(-35.9845742172474,0.815766203738364,
306.595619207947));
#12082=CARTESIAN_POINT('Ctrl Pts',(-36.0105706539352,0.740911841440301,
306.600914331614));
#12083=CARTESIAN_POINT('Ctrl Pts',(-36.0327666015562,0.664913755407971,
306.606209455282));
#12084=CARTESIAN_POINT('Ctrl Pts',(-36.0549533461896,0.588947180057778,
306.61150238346));
#12085=CARTESIAN_POINT('Ctrl Pts',(-36.0733426017308,0.511838276606008,
306.616795311638));
#12086=CARTESIAN_POINT('Ctrl Pts',(-36.08783034275,0.434001960473747,306.622088239817));
#12087=CARTESIAN_POINT('Ctrl Pts',(-36.1023225761047,0.356141508981568,
306.627382809218));
#12088=CARTESIAN_POINT('Ctrl Pts',(-36.1129107851658,0.277553657859791,
306.632677378619));
#12089=CARTESIAN_POINT('Ctrl Pts',(-36.1195421286928,0.198663311545526,
306.63797194802));
#12090=CARTESIAN_POINT('Ctrl Pts',(-36.1251524719885,0.131919381942699,
306.642451334712));
#12091=CARTESIAN_POINT('Ctrl Pts',(-36.1279314652037,0.0649592490742431,
306.646930721403));
#12092=CARTESIAN_POINT('Ctrl Pts',(-36.12787621691,-0.00195816148385779,
306.651410108095));
#12093=CARTESIAN_POINT('Ctrl Pts',(-36.1261829184293,-0.00197080147836691,
306.651411048457));
#12094=CARTESIAN_POINT('Ctrl Pts',(-36.128116703496,-0.251180220789445,
306.668104687931));
#12095=CARTESIAN_POINT('Ctrl Pts',(-35.9771376933501,-1.28886751917914,
306.737768758128));
#12096=CARTESIAN_POINT('Ctrl Pts',(-34.4707053354124,-2.71176214819284,
306.860403259048));
#12097=CARTESIAN_POINT('Ctrl Pts',(-31.8635119515384,-2.06936810284668,
307.019314551217));
#12098=CARTESIAN_POINT('Ctrl Pts',(-31.0125546758027,0.408963281941028,
307.174390069647));
#12099=CARTESIAN_POINT('Ctrl Pts',(-32.0218921613136,1.77375560660345,307.276495157355));
#12100=CARTESIAN_POINT('Ctrl Pts',(-32.6683119391961,2.11155019427352,307.325629814339));
#12101=CARTESIAN_POINT('Origin',(-33.7561270252576,0.,302.151410108095));
#12102=CARTESIAN_POINT('',(-32.6699490794739,2.10841540797657,308.52497223169));
#12103=CARTESIAN_POINT('',(-32.6699491752354,2.10841545730937,308.326094215555));
#12104=CARTESIAN_POINT('',(-32.6699490794746,2.10841540797695,302.151410108095));
#12105=CARTESIAN_POINT('Ctrl Pts',(-32.6699490794745,2.10841540797688,308.52497223169));
#12106=CARTESIAN_POINT('Ctrl Pts',(-32.6697542748568,2.10831505181432,308.524957834865));
#12107=CARTESIAN_POINT('Ctrl Pts',(-32.6695594840382,2.10821466859727,308.524943437104));
#12108=CARTESIAN_POINT('Ctrl Pts',(-32.648369882537,2.09729113332925,308.523377016956));
#12109=CARTESIAN_POINT('Ctrl Pts',(-32.6275385802355,2.0861553247313,308.52181433451));
#12110=CARTESIAN_POINT('Ctrl Pts',(-32.5873096832505,2.06387123670633,308.518749964238));
#12111=CARTESIAN_POINT('Ctrl Pts',(-32.5678966164551,2.05275592723339,308.51724958258));
#12112=CARTESIAN_POINT('Ctrl Pts',(-32.521426213119,2.02526837387622,308.51360388372));
#12113=CARTESIAN_POINT('Ctrl Pts',(-32.4945341167153,2.00862670649824,308.511448912638));
#12114=CARTESIAN_POINT('Ctrl Pts',(-32.3989261999558,1.94678408147741,308.503618667244));
#12115=CARTESIAN_POINT('Ctrl Pts',(-32.3322464250881,1.89855831636061,308.497833801045));
#12116=CARTESIAN_POINT('Ctrl Pts',(-32.2579515648505,1.83870659476065,308.491006349664));
#12117=CARTESIAN_POINT('Ctrl Pts',(-32.2477606154721,1.83035581706245,308.490061111339));
#12118=CARTESIAN_POINT('Ctrl Pts',(-32.0926299878261,1.70106156965988,308.475539419776));
#12119=CARTESIAN_POINT('Ctrl Pts',(-31.9625763998646,1.56333137965069,308.461499449945));
#12120=CARTESIAN_POINT('Ctrl Pts',(-31.8284628308755,1.38226118142892,308.445515867498));
#12121=CARTESIAN_POINT('Ctrl Pts',(-31.807379373289,1.35237500724561,308.44295086956));
#12122=CARTESIAN_POINT('Ctrl Pts',(-31.7779592063255,1.30855373612376,308.439306908925));
#12123=CARTESIAN_POINT('Ctrl Pts',(-31.7690620906967,1.29500339137565,308.438195816581));
#12124=CARTESIAN_POINT('Ctrl Pts',(-31.7535476924234,1.27083849590288,308.43624344493));
#12125=CARTESIAN_POINT('Ctrl Pts',(-31.7468745208969,1.26026142564978,308.435398700216));
#12126=CARTESIAN_POINT('Ctrl Pts',(-31.73193690934,1.23616482292314,308.433496277736));
#12127=CARTESIAN_POINT('Ctrl Pts',(-31.7237238573915,1.22261461344489,308.432441845368));
#12128=CARTESIAN_POINT('Ctrl Pts',(-31.6981014985519,1.17937006123461,308.429121724834));
#12129=CARTESIAN_POINT('Ctrl Pts',(-31.6812016812521,1.14937718787041,308.426885573243));
#12130=CARTESIAN_POINT('Ctrl Pts',(-31.5714809950463,0.944337749136008,
308.411969255072));
#12131=CARTESIAN_POINT('Ctrl Pts',(-31.5002498458649,0.758609238711452,
308.400196080818));
#12132=CARTESIAN_POINT('Ctrl Pts',(-31.4316686244342,0.479619053799077,
308.382355799246));
#12133=CARTESIAN_POINT('Ctrl Pts',(-31.4152906630639,0.391948818370953,
308.376738581987));
#12134=CARTESIAN_POINT('Ctrl Pts',(-31.3998323773657,0.272169253142799,
308.36891803522));
#12135=CARTESIAN_POINT('Ctrl Pts',(-31.3964091478656,0.240690575271756,
308.366849687097));
#12136=CARTESIAN_POINT('Ctrl Pts',(-31.3916242167409,0.186642134752707,
308.363271045692));
#12137=CARTESIAN_POINT('Ctrl Pts',(-31.3899531614768,0.164103638394417,
308.361770641594));
#12138=CARTESIAN_POINT('Ctrl Pts',(-31.3871922228285,0.1179234957643,308.358678194116));
#12139=CARTESIAN_POINT('Ctrl Pts',(-31.3861336141789,0.0942826059095021,
308.357085341973));
#12140=CARTESIAN_POINT('Ctrl Pts',(-31.3843168457758,0.0333032031595571,
308.352949865781));
#12141=CARTESIAN_POINT('Ctrl Pts',(-31.384086551998,-0.00404323980376545,
308.350391098596));
#12142=CARTESIAN_POINT('Ctrl Pts',(-31.3883276229169,-0.247101946770624,
308.333559524211));
#12143=CARTESIAN_POINT('Ctrl Pts',(-31.4186730931841,-0.451453949153685,
308.318463712881));
#12144=CARTESIAN_POINT('Ctrl Pts',(-31.4998741205617,-0.736743829507453,
308.296871488298));
#12145=CARTESIAN_POINT('Ctrl Pts',(-31.5297829911895,-0.822717608745344,
308.290310819784));
#12146=CARTESIAN_POINT('Ctrl Pts',(-31.5727648889355,-0.926600496625176,
308.282472474566));
#12147=CARTESIAN_POINT('Ctrl Pts',(-31.5812396044316,-0.946321027588535,
308.280988738936));
#12148=CARTESIAN_POINT('Ctrl Pts',(-31.5953968071521,-0.978069430686514,
308.278610069112));
#12149=CARTESIAN_POINT('Ctrl Pts',(-31.6009146153508,-0.990168863814282,
308.277705939843));
#12150=CARTESIAN_POINT('Ctrl Pts',(-31.6122004359407,-1.01437500641261,
308.275902892951));
#12151=CARTESIAN_POINT('Ctrl Pts',(-31.6179699313795,-1.02648046168159,
308.275004101913));
#12152=CARTESIAN_POINT('Ctrl Pts',(-31.6334714183632,-1.05830754001571,
308.272647047806));
#12153=CARTESIAN_POINT('Ctrl Pts',(-31.6433758114949,-1.07794437218729,
308.271198920616));
#12154=CARTESIAN_POINT('Ctrl Pts',(-31.7014952220605,-1.18929464050435,
308.263006364641));
#12155=CARTESIAN_POINT('Ctrl Pts',(-31.7554116824241,-1.27791894335982,
308.256557735778));
#12156=CARTESIAN_POINT('Ctrl Pts',(-31.8908308417353,-1.47081793333816,
308.242046205086));
#12157=CARTESIAN_POINT('Ctrl Pts',(-31.9755938651227,-1.57236639485723,
308.234042502347));
#12158=CARTESIAN_POINT('Ctrl Pts',(-32.121613255749,-1.72026352478538,308.221054644192));
#12159=CARTESIAN_POINT('Ctrl Pts',(-32.1774096619966,-1.77160708026099,
308.216247889956));
#12160=CARTESIAN_POINT('Ctrl Pts',(-32.2586921250765,-1.83950944134362,
308.209375063999));
#12161=CARTESIAN_POINT('Ctrl Pts',(-32.2821853972595,-1.85838699053612,
308.207402925673));
#12162=CARTESIAN_POINT('Ctrl Pts',(-32.323726049381,-1.89048288397758,308.203936122047));
#12163=CARTESIAN_POINT('Ctrl Pts',(-32.3416129004449,-1.90390331228865,
308.202449703314));
#12164=CARTESIAN_POINT('Ctrl Pts',(-32.3792454311392,-1.93131579081057,
308.199333855758));
#12165=CARTESIAN_POINT('Ctrl Pts',(-32.3990207738363,-1.94526248993868,
308.197702899811));
#12166=CARTESIAN_POINT('Ctrl Pts',(-32.4520654778456,-1.9814700983897,308.193342930609));
#12167=CARTESIAN_POINT('Ctrl Pts',(-32.4856896329674,-2.0031946394492,308.190594260586));
#12168=CARTESIAN_POINT('Ctrl Pts',(-32.65372404966,-2.1058290152217,308.176923033223));
#12169=CARTESIAN_POINT('Ctrl Pts',(-32.7953644104614,-2.1741040331218,308.165562217286));
#12170=CARTESIAN_POINT('Ctrl Pts',(-33.0281375237343,-2.25909403744493,
308.14746299889));
#12171=CARTESIAN_POINT('Ctrl Pts',(-33.115322881501,-2.28535468439157,308.140810319842));
#12172=CARTESIAN_POINT('Ctrl Pts',(-33.2528059330067,-2.31827624780975,
308.130680020555));
#12173=CARTESIAN_POINT('Ctrl Pts',(-33.3021729215608,-2.32844655809023,
308.12711337567));
#12174=CARTESIAN_POINT('Ctrl Pts',(-33.3697585590679,-2.34013856792791,
308.122358014188));
#12175=CARTESIAN_POINT('Ctrl Pts',(-33.3877227448265,-2.34303381254994,
308.121106214314));
#12176=CARTESIAN_POINT('Ctrl Pts',(-33.4182710689383,-2.34759717188068,
308.119000127986));
#12177=CARTESIAN_POINT('Ctrl Pts',(-33.4308382168061,-2.34937148003678,
308.118140229852));
#12178=CARTESIAN_POINT('Ctrl Pts',(-33.4577927696138,-2.35295664436021,
308.116310374752));
#12179=CARTESIAN_POINT('Ctrl Pts',(-33.4721834001099,-2.35473657625174,
308.115342083902));
#12180=CARTESIAN_POINT('Ctrl Pts',(-33.5128952934578,-2.3593934419375,308.11262481515));
#12181=CARTESIAN_POINT('Ctrl Pts',(-33.53925055855,-2.36196186042849,308.110891781249));
#12182=CARTESIAN_POINT('Ctrl Pts',(-33.6643944532447,-2.3720451162905,308.102762338388));
#12183=CARTESIAN_POINT('Ctrl Pts',(-33.7635567364719,-2.37380745681212,
308.09661197928));
#12184=CARTESIAN_POINT('Ctrl Pts',(-33.9889953647975,-2.36368180310672,
308.082730119426));
#12185=CARTESIAN_POINT('Ctrl Pts',(-34.114781457606,-2.34788956288181,308.075048713537));
#12186=CARTESIAN_POINT('Ctrl Pts',(-34.3139541748837,-2.30649818637312,
308.062343340631));
#12187=CARTESIAN_POINT('Ctrl Pts',(-34.3883919737379,-2.28721321442363,
308.057471349542));
#12188=CARTESIAN_POINT('Ctrl Pts',(-34.4906580942736,-2.25534443709275,
308.050521765373));
#12189=CARTESIAN_POINT('Ctrl Pts',(-34.5193825206474,-2.24578612796657,
308.048541113089));
#12190=CARTESIAN_POINT('Ctrl Pts',(-34.5690119733194,-2.22820937687997,
308.045064525627));
#12191=CARTESIAN_POINT('Ctrl Pts',(-34.5900013818312,-2.22043970079052,
308.043576980269));
#12192=CARTESIAN_POINT('Ctrl Pts',(-34.6333985245347,-2.20367322980368,
308.040463796503));
#12193=CARTESIAN_POINT('Ctrl Pts',(-34.6557850189734,-2.19462899060574,
308.038836700144));
#12194=CARTESIAN_POINT('Ctrl Pts',(-34.7146582443577,-2.1697918044283,308.034499482581));
#12195=CARTESIAN_POINT('Ctrl Pts',(-34.750891256558,-2.15342108385763,308.031770072265));
#12196=CARTESIAN_POINT('Ctrl Pts',(-34.9321409666564,-2.06597867834001,
308.017801287286));
#12197=CARTESIAN_POINT('Ctrl Pts',(-35.0700184466392,-1.98114859418881,
308.006093034955));
#12198=CARTESIAN_POINT('Ctrl Pts',(-35.2681226563116,-1.82943339383273,
307.987866453835));
#12199=CARTESIAN_POINT('Ctrl Pts',(-35.3350220046007,-1.77201844289353,
307.981430235382));
#12200=CARTESIAN_POINT('Ctrl Pts',(-35.4342506891282,-1.67676612268595,
307.971579549188));
#12201=CARTESIAN_POINT('Ctrl Pts',(-35.4688498730938,-1.64140942128715,
307.968080914963));
#12202=CARTESIAN_POINT('Ctrl Pts',(-35.5145546470336,-1.59168376047633,
307.963399416128));
#12203=CARTESIAN_POINT('Ctrl Pts',(-35.5266364951789,-1.57823355756364,
307.962155852577));
#12204=CARTESIAN_POINT('Ctrl Pts',(-35.5469252043895,-1.55512076283722,
307.960059141527));
#12205=CARTESIAN_POINT('Ctrl Pts',(-35.5552103448498,-1.54552837104443,
307.959200507061));
#12206=CARTESIAN_POINT('Ctrl Pts',(-35.5728457011268,-1.52477645431676,
307.957368134114));
#12207=CARTESIAN_POINT('Ctrl Pts',(-35.5821706416015,-1.51359661794947,
307.95639613445));
#12208=CARTESIAN_POINT('Ctrl Pts',(-35.6083369626702,-1.481631536107,307.953657381288));
#12209=CARTESIAN_POINT('Ctrl Pts',(-35.6249310273757,-1.46064554547021,
307.951906969884));
#12210=CARTESIAN_POINT('Ctrl Pts',(-35.7049666369477,-1.35582950369665,
307.943370944638));
#12211=CARTESIAN_POINT('Ctrl Pts',(-35.7631474918,-1.26811793654532,307.9368633105));
#12212=CARTESIAN_POINT('Ctrl Pts',(-35.8634475536584,-1.09261434813488,
307.924444136605));
#12213=CARTESIAN_POINT('Ctrl Pts',(-35.9063626397152,-1.00553089679297,
307.918536730961));
#12214=CARTESIAN_POINT('Ctrl Pts',(-35.9805724135404,-0.828307100562886,
307.90663443121));
#12215=CARTESIAN_POINT('Ctrl Pts',(-36.012002414096,-0.738426161484981,
307.900654107954));
#12216=CARTESIAN_POINT('Ctrl Pts',(-36.0467432470147,-0.615885605863798,
307.892412700175));
#12217=CARTESIAN_POINT('Ctrl Pts',(-36.0549041411989,-0.584689115442946,
307.89030768033));
#12218=CARTESIAN_POINT('Ctrl Pts',(-36.0677220082109,-0.531264477556838,
307.886685800129));
#12219=CARTESIAN_POINT('Ctrl Pts',(-36.0727004682386,-0.509117602033948,
307.885179470436));
#12220=CARTESIAN_POINT('Ctrl Pts',(-36.0816130422755,-0.466628341438866,
307.882278619619));
#12221=CARTESIAN_POINT('Ctrl Pts',(-36.0855999907097,-0.446299092795844,
307.880885948514));
#12222=CARTESIAN_POINT('Ctrl Pts',(-36.0954232086945,-0.392487527835203,
307.877185802047));
#12223=CARTESIAN_POINT('Ctrl Pts',(-36.1008067832265,-0.358928567925944,
307.874864217193));
#12224=CARTESIAN_POINT('Ctrl Pts',(-36.1204886453171,-0.216770304780468,
307.86496553811));
#12225=CARTESIAN_POINT('Ctrl Pts',(-36.1279742159633,-0.107378564969787,
307.857182146614));
#12226=CARTESIAN_POINT('Ctrl Pts',(-36.1277925564576,0.0953097255528812,
307.842518464619));
#12227=CARTESIAN_POINT('Ctrl Pts',(-36.1222173954371,0.188405761762015,
307.835691019819));
#12228=CARTESIAN_POINT('Ctrl Pts',(-36.0993641809586,0.379986546714878,
307.821623522208));
#12229=CARTESIAN_POINT('Ctrl Pts',(-36.0813084448988,0.478210813311289,
307.814401901211));
#12230=CARTESIAN_POINT('Ctrl Pts',(-36.0517918752457,0.596324959568578,
307.805907049349));
#12231=CARTESIAN_POINT('Ctrl Pts',(-36.0461703700952,0.617561435737019,
307.80438752565));
#12232=CARTESIAN_POINT('Ctrl Pts',(-36.0366446524408,0.651626489706044,
307.801966016027));
#12233=CARTESIAN_POINT('Ctrl Pts',(-36.0329254416588,0.664504870916143,
307.801054257331));
#12234=CARTESIAN_POINT('Ctrl Pts',(-36.0252980093427,0.690100042069758,
307.799250520573));
#12235=CARTESIAN_POINT('Ctrl Pts',(-36.0213915898061,0.702816829367536,
307.79835849386));
#12236=CARTESIAN_POINT('Ctrl Pts',(-36.0108963036553,0.735985892266726,
307.796041053341));
#12237=CARTESIAN_POINT('Ctrl Pts',(-36.0041359747943,0.756383220297852,
307.794625165464));
#12238=CARTESIAN_POINT('Ctrl Pts',(-35.9671486370035,0.863102681964889,
307.787251906237));
#12239=CARTESIAN_POINT('Ctrl Pts',(-35.9322211667796,0.947724043275812,
307.78152415316));
#12240=CARTESIAN_POINT('Ctrl Pts',(-35.8035560887079,1.21456084626016,307.763218125622));
#12241=CARTESIAN_POINT('Ctrl Pts',(-35.6911234696286,1.3866900089454,307.750939954969));
#12242=CARTESIAN_POINT('Ctrl Pts',(-35.5335694788711,1.57076609099005,307.735360177558));
#12243=CARTESIAN_POINT('Ctrl Pts',(-35.5084820867311,1.59870549959886,307.732921535792));
#12244=CARTESIAN_POINT('Ctrl Pts',(-35.4664919964326,1.64329291781381,307.728898175018));
#12245=CARTESIAN_POINT('Ctrl Pts',(-35.4499835291377,1.6603041961926,307.727330306133));
#12246=CARTESIAN_POINT('Ctrl Pts',(-35.4172585068807,1.69302983611128,307.724247090564));
#12247=CARTESIAN_POINT('Ctrl Pts',(-35.4010669959496,1.70876571152136,307.722732945937));
#12248=CARTESIAN_POINT('Ctrl Pts',(-35.3617311550341,1.74591741009388,307.719079718324));
#12249=CARTESIAN_POINT('Ctrl Pts',(-35.3383801091086,1.76710702442154,307.716931284295));
#12250=CARTESIAN_POINT('Ctrl Pts',(-35.2483967040069,1.84554763981705,307.70872331868));
#12251=CARTESIAN_POINT('Ctrl Pts',(-35.179030927775,1.89954102569049,307.702535659541));
#12252=CARTESIAN_POINT('Ctrl Pts',(-34.9516381436544,2.0570853809518,307.682698436166));
#12253=CARTESIAN_POINT('Ctrl Pts',(-34.7841681281559,2.14568684717222,307.668662132311));
#12254=CARTESIAN_POINT('Ctrl Pts',(-34.5695888448959,2.22826602888145,307.652279204754));
#12255=CARTESIAN_POINT('Ctrl Pts',(-34.5308239999495,2.24203806835419,307.649382093788));
#12256=CARTESIAN_POINT('Ctrl Pts',(-34.4767343348253,2.25968395395205,307.645443157625));
#12257=CARTESIAN_POINT('Ctrl Pts',(-34.4617018226034,2.2644228195073,307.64435935515));
#12258=CARTESIAN_POINT('Ctrl Pts',(-34.4345130235691,2.27269679545539,307.642420089707));
#12259=CARTESIAN_POINT('Ctrl Pts',(-34.422373593407,2.27628509388628,307.641561740739));
#12260=CARTESIAN_POINT('Ctrl Pts',(-34.3965739802381,2.28368712128925,307.639754056385));
#12261=CARTESIAN_POINT('Ctrl Pts',(-34.382907431527,2.28747579621743,307.638806110259));
#12262=CARTESIAN_POINT('Ctrl Pts',(-34.3444059876715,2.29777829054088,307.636160367355));
#12263=CARTESIAN_POINT('Ctrl Pts',(-34.3194973208564,2.30401199038756,307.634477555899));
#12264=CARTESIAN_POINT('Ctrl Pts',(-34.1523543874522,2.34296868964753,307.623347343232));
#12265=CARTESIAN_POINT('Ctrl Pts',(-34.0074444705203,2.36291108848683,307.614463716015));
#12266=CARTESIAN_POINT('Ctrl Pts',(-33.7245743813617,2.37550356416093,307.597110497572));
#12267=CARTESIAN_POINT('Ctrl Pts',(-33.5872869385353,2.3697047077334,307.588677199415));
#12268=CARTESIAN_POINT('Ctrl Pts',(-33.4113105662334,2.34689664467568,307.577299817156));
#12269=CARTESIAN_POINT('Ctrl Pts',(-33.3714842033524,2.34069900728107,307.574688295764));
#12270=CARTESIAN_POINT('Ctrl Pts',(-33.3079754915257,2.32915144502778,307.570454291191));
#12271=CARTESIAN_POINT('Ctrl Pts',(-33.2841828526557,2.32444721938452,307.568852318163));
#12272=CARTESIAN_POINT('Ctrl Pts',(-33.2386181067272,2.31470986710964,307.565751938187));
#12273=CARTESIAN_POINT('Ctrl Pts',(-33.2168367007447,2.30973226508669,307.564255465589));
#12274=CARTESIAN_POINT('Ctrl Pts',(-33.1659765892476,2.29735081885887,307.560725816924));
#12275=CARTESIAN_POINT('Ctrl Pts',(-33.1369622148869,2.28970153411024,307.558684914724));
#12276=CARTESIAN_POINT('Ctrl Pts',(-33.0361861696619,2.26107769404405,307.551496810703));
#12277=CARTESIAN_POINT('Ctrl Pts',(-32.9652838867656,2.23726445359715,307.54626005412));
#12278=CARTESIAN_POINT('Ctrl Pts',(-32.8186507790181,2.18017441547123,307.535050914851));
#12279=CARTESIAN_POINT('Ctrl Pts',(-32.7433222279446,2.14621455870658,307.529068256111));
#12280=CARTESIAN_POINT('Ctrl Pts',(-32.669948905789,2.10841531850051,307.52304986714));
#12281=CARTESIAN_POINT('',(-36.1316341613132,-0.000310224732309534,307.651557338406));
#12282=CARTESIAN_POINT('Ctrl Pts',(-32.6683119391961,2.11155019427352,307.325629814339));
#12283=CARTESIAN_POINT('Ctrl Pts',(-32.7187757087736,2.13792065634783,307.329465588078));
#12284=CARTESIAN_POINT('Ctrl Pts',(-33.480627950877,2.49966777931651,307.38627179254));
#12285=CARTESIAN_POINT('Ctrl Pts',(-35.3072153547382,2.32488896510995,307.494865049128));
#12286=CARTESIAN_POINT('Ctrl Pts',(-36.1304027123948,0.767986961440899,
307.599622531977));
#12287=CARTESIAN_POINT('Ctrl Pts',(-36.1318916699647,-0.000319976874305989,
307.651409584103));
#12288=CARTESIAN_POINT('Ctrl Pts',(-36.127877019312,-0.000167937542783692,
307.653713125769));
#12289=CARTESIAN_POINT('Ctrl Pts',(-36.1278765090554,-0.00737419368197688,
307.654208311306));
#12290=CARTESIAN_POINT('Ctrl Pts',(-36.127843155871,-0.0145805378433049,
307.654701857024));
#12291=CARTESIAN_POINT('Ctrl Pts',(-36.127694085241,-0.0308079898488567,
307.655809365293));
#12292=CARTESIAN_POINT('Ctrl Pts',(-36.1275597397538,-0.039828880661449,
307.656422337782));
#12293=CARTESIAN_POINT('Ctrl Pts',(-36.1271115390896,-0.0615856206795041,
307.657893862826));
#12294=CARTESIAN_POINT('Ctrl Pts',(-36.1267465408413,-0.0743200882215176,
307.658749416002));
#12295=CARTESIAN_POINT('Ctrl Pts',(-36.1255781386497,-0.106132282250148,
307.660873635551));
#12296=CARTESIAN_POINT('Ctrl Pts',(-36.1246469054167,-0.125204933390442,
307.662135473233));
#12297=CARTESIAN_POINT('Ctrl Pts',(-36.1199726224132,-0.201908932090859,
307.667170518765));
#12298=CARTESIAN_POINT('Ctrl Pts',(-36.1143553003309,-0.259410452491916,
307.67085503912));
#12299=CARTESIAN_POINT('Ctrl Pts',(-36.0993672545264,-0.370666356698195,
307.677907012708));
#12300=CARTESIAN_POINT('Ctrl Pts',(-36.090231052281,-0.424413946499034,
307.681278500044));
#12301=CARTESIAN_POINT('Ctrl Pts',(-36.0790227014757,-0.478910244553418,
307.684701385748));
#12302=CARTESIAN_POINT('Ctrl Pts',(-36.078793770254,-0.480019308592317,
307.684771047274));
#12303=CARTESIAN_POINT('Ctrl Pts',(-36.0783012437081,-0.482396766123027,
307.684920382481));
#12304=CARTESIAN_POINT('Ctrl Pts',(-36.0780374032698,-0.483665108608161,
307.685000053608));
#12305=CARTESIAN_POINT('Ctrl Pts',(-36.0774696446138,-0.486383285530192,
307.685170803283));
#12306=CARTESIAN_POINT('Ctrl Pts',(-36.0771654069789,-0.487833052861174,
307.685261878618));
#12307=CARTESIAN_POINT('Ctrl Pts',(-36.0765105376764,-0.490939185927556,
307.685457018683));
#12308=CARTESIAN_POINT('Ctrl Pts',(-36.0761594902127,-0.492595463383139,
307.685561079404));
#12309=CARTESIAN_POINT('Ctrl Pts',(-36.0596340523472,-0.570154625741113,
307.690434331927));
#12310=CARTESIAN_POINT('Ctrl Pts',(-36.0397457800762,-0.64521800625907,
307.695168606122));
#12311=CARTESIAN_POINT('Ctrl Pts',(-35.981991286292,-0.826718830723631,
307.706901769611));
#12312=CARTESIAN_POINT('Ctrl Pts',(-35.9401401747814,-0.931674806330502,
307.71394249447));
#12313=CARTESIAN_POINT('Ctrl Pts',(-35.8763376098401,-1.06350127103369,
307.723402362815));
#12314=CARTESIAN_POINT('Ctrl Pts',(-35.8610534552305,-1.09344063211769,
307.725593587552));
#12315=CARTESIAN_POINT('Ctrl Pts',(-35.8342749221447,-1.14325228371779,
307.729317980128));
#12316=CARTESIAN_POINT('Ctrl Pts',(-35.8231186675002,-1.16330131682555,
307.730839070142));
#12317=CARTESIAN_POINT('Ctrl Pts',(-35.8001138563068,-1.20326756977821,
307.733917633036));
#12318=CARTESIAN_POINT('Ctrl Pts',(-35.7882607546979,-1.2231792384507,307.735475147773));
#12319=CARTESIAN_POINT('Ctrl Pts',(-35.7578663628417,-1.27257640502601,
307.739400647811));
#12320=CARTESIAN_POINT('Ctrl Pts',(-35.7389642822171,-1.30183227410116,
307.741781708271));
#12321=CARTESIAN_POINT('Ctrl Pts',(-35.6441790637803,-1.44168144016217,
307.753446055091));
#12322=CARTESIAN_POINT('Ctrl Pts',(-35.5596630212636,-1.5461026355357,307.763051597278));
#12323=CARTESIAN_POINT('Ctrl Pts',(-35.3868766020232,-1.72602583638157,
307.781207693843));
#12324=CARTESIAN_POINT('Ctrl Pts',(-35.3009953850314,-1.80330029230458,
307.789689672557));
#12325=CARTESIAN_POINT('Ctrl Pts',(-35.1645491797456,-1.90914359139318,
307.802112625275));
#12326=CARTESIAN_POINT('Ctrl Pts',(-35.1180058033821,-1.942619249809,307.806184784382));
#12327=CARTESIAN_POINT('Ctrl Pts',(-35.0544872931942,-1.98489775771553,
307.811482730365));
#12328=CARTESIAN_POINT('Ctrl Pts',(-35.0385566986853,-1.99522747699303,
307.812790575262));
#12329=CARTESIAN_POINT('Ctrl Pts',(-35.0116667774051,-2.01220830143521,
307.814961185446));
#12330=CARTESIAN_POINT('Ctrl Pts',(-35.0007746883969,-2.01896373041983,
307.815830413431));
#12331=CARTESIAN_POINT('Ctrl Pts',(-34.9777437091783,-2.03299063665592,
307.817646726324));
#12332=CARTESIAN_POINT('Ctrl Pts',(-34.9655936938365,-2.04024230288451,
307.818592598252));
#12333=CARTESIAN_POINT('Ctrl Pts',(-34.9313500427877,-2.0602670087037,307.821226206858));
#12334=CARTESIAN_POINT('Ctrl Pts',(-34.9091133892519,-2.0727932511646,307.822899176504));
#12335=CARTESIAN_POINT('Ctrl Pts',(-34.7604451424701,-2.15340731666415,
307.833869391093));
#12336=CARTESIAN_POINT('Ctrl Pts',(-34.6282403864116,-2.21025942671556,
307.8426198623));
#12337=CARTESIAN_POINT('Ctrl Pts',(-34.3963596429151,-2.28590358685133,
307.857566676457));
#12338=CARTESIAN_POINT('Ctrl Pts',(-34.2991573293271,-2.3109239275784,307.863719024815));
#12339=CARTESIAN_POINT('Ctrl Pts',(-34.1564474395464,-2.33815489656479,
307.872854373876));
#12340=CARTESIAN_POINT('Ctrl Pts',(-34.111997372899,-2.34533167942639,307.875712989716));
#12341=CARTESIAN_POINT('Ctrl Pts',(-34.0302851279116,-2.35614832473346,
307.881013752131));
#12342=CARTESIAN_POINT('Ctrl Pts',(-33.993089164764,-2.36017929145379,307.883443848311));
#12343=CARTESIAN_POINT('Ctrl Pts',(-33.9322230478898,-2.36532213622309,
307.887456743865));
#12344=CARTESIAN_POINT('Ctrl Pts',(-33.9086033020265,-2.3669620896453,307.889022865845));
#12345=CARTESIAN_POINT('Ctrl Pts',(-33.8626596055415,-2.3694615032158,307.892088353743));
#12346=CARTESIAN_POINT('Ctrl Pts',(-33.8403402065243,-2.37035969565154,
307.893586332386));
#12347=CARTESIAN_POINT('Ctrl Pts',(-33.7865919296176,-2.37176260438227,
307.897216290942));
#12348=CARTESIAN_POINT('Ctrl Pts',(-33.7551599587579,-2.37195802260147,
307.899357717033));
#12349=CARTESIAN_POINT('Ctrl Pts',(-33.6434878640738,-2.37043270973191,
307.90703586961));
#12350=CARTESIAN_POINT('Ctrl Pts',(-33.5633571785347,-2.36526448474291,
307.91267628221));
#12351=CARTESIAN_POINT('Ctrl Pts',(-33.4661784296475,-2.35402574484011,
307.91967042979));
#12352=CARTESIAN_POINT('Ctrl Pts',(-33.4487303293756,-2.35181092913946,
307.920932167285));
#12353=CARTESIAN_POINT('Ctrl Pts',(-33.2824230179605,-2.3288179950122,307.93301293664));
#12354=CARTESIAN_POINT('Ctrl Pts',(-33.1358408946272,-2.29412952272418,
307.944108376364));
#12355=CARTESIAN_POINT('Ctrl Pts',(-32.9322345423204,-2.22499208796223,
307.95963210317));
#12356=CARTESIAN_POINT('Ctrl Pts',(-32.8718095199361,-2.2016749775241,307.964249384));
#12357=CARTESIAN_POINT('Ctrl Pts',(-32.7943267188082,-2.16806981427336,
307.970121008768));
#12358=CARTESIAN_POINT('Ctrl Pts',(-32.7763418367738,-2.16000175882924,
307.971480292437));
#12359=CARTESIAN_POINT('Ctrl Pts',(-32.746713721265,-2.14626430107095,307.973711091706));
#12360=CARTESIAN_POINT('Ctrl Pts',(-32.7350128372068,-2.14072219474714,
307.974589856524));
#12361=CARTESIAN_POINT('Ctrl Pts',(-32.7108570364416,-2.12903770062934,
307.976398568031));
#12362=CARTESIAN_POINT('Ctrl Pts',(-32.6984097069005,-2.12288129181267,
307.977327663037));
#12363=CARTESIAN_POINT('Ctrl Pts',(-32.6643732758007,-2.10567328683639,
307.979862127884));
#12364=CARTESIAN_POINT('Ctrl Pts',(-32.6428978486329,-2.09439899572613,
307.98145447193));
#12365=CARTESIAN_POINT('Ctrl Pts',(-32.484685188987,-2.00821831807319,307.993163086215));
#12366=CARTESIAN_POINT('Ctrl Pts',(-32.3554405212278,-1.92031132432452,
308.002619572892));
#12367=CARTESIAN_POINT('Ctrl Pts',(-32.1314981972803,-1.73327106113856,
308.020509619051));
#12368=CARTESIAN_POINT('Ctrl Pts',(-32.0349323387032,-1.63741579241115,
308.028885978213));
#12369=CARTESIAN_POINT('Ctrl Pts',(-31.9230844722645,-1.50550078619912,
308.040011618715));
#12370=CARTESIAN_POINT('Ctrl Pts',(-31.8997341261551,-1.47661192513993,
308.042424881406));
#12371=CARTESIAN_POINT('Ctrl Pts',(-31.8626584672837,-1.42847223646105,
308.046417321166));
#12372=CARTESIAN_POINT('Ctrl Pts',(-31.8485251077224,-1.40954282181255,
308.047980161213));
#12373=CARTESIAN_POINT('Ctrl Pts',(-31.8215657861463,-1.37228681089711,
308.05104440554));
#12374=CARTESIAN_POINT('Ctrl Pts',(-31.8087116591879,-1.3539836083857,308.0525444976));
#12375=CARTESIAN_POINT('Ctrl Pts',(-31.7783218049435,-1.30938287163757,
308.0561887144));
#12376=CARTESIAN_POINT('Ctrl Pts',(-31.7610496040051,-1.28291188658631,
308.058342475401));
#12377=CARTESIAN_POINT('Ctrl Pts',(-31.7008491811293,-1.18649309442998,
308.066159037659));
#12378=CARTESIAN_POINT('Ctrl Pts',(-31.6610332297251,-1.11468030765325,
308.071930892358));
#12379=CARTESIAN_POINT('Ctrl Pts',(-31.6186200939947,-1.02784966403373,
308.078845886496));
#12380=CARTESIAN_POINT('Ctrl Pts',(-31.6123394703698,-1.01468503536244,
308.079892524471));
#12381=CARTESIAN_POINT('Ctrl Pts',(-31.5268419288237,-0.831138533660723,
308.094458681905));
#12382=CARTESIAN_POINT('Ctrl Pts',(-31.4680283704042,-0.652000157306974,
308.108431684514));
#12383=CARTESIAN_POINT('Ctrl Pts',(-31.4238007818546,-0.432172798124201,
308.124334417911));
#12384=CARTESIAN_POINT('Ctrl Pts',(-31.4174515582709,-0.396379160406,308.126883415748));
#12385=CARTESIAN_POINT('Ctrl Pts',(-31.4094695078673,-0.344467816460916,
308.130509128568));
#12386=CARTESIAN_POINT('Ctrl Pts',(-31.407175258702,-0.328458850252923,
308.131617553476));
#12387=CARTESIAN_POINT('Ctrl Pts',(-31.403397644424,-0.300031478304804,
308.133567134708));
#12388=CARTESIAN_POINT('Ctrl Pts',(-31.4018485040756,-0.287623177273709,
308.134411715774));
#12389=CARTESIAN_POINT('Ctrl Pts',(-31.3985552189583,-0.259432677195143,
308.13631611495));
#12390=CARTESIAN_POINT('Ctrl Pts',(-31.396871305245,-0.243644451177669,
308.137372650129));
#12391=CARTESIAN_POINT('Ctrl Pts',(-31.3920209420462,-0.193387045003184,
308.140707381243));
#12392=CARTESIAN_POINT('Ctrl Pts',(-31.3894502688549,-0.158863307025585,
308.142955670595));
#12393=CARTESIAN_POINT('Ctrl Pts',(-31.3772659998629,0.0733154598678785,
308.157865437777));
#12394=CARTESIAN_POINT('Ctrl Pts',(-31.3916651894792,0.271464154717219,
308.169624849468));
#12395=CARTESIAN_POINT('Ctrl Pts',(-31.4480025886223,0.552898853618975,
308.187448133103));
#12396=CARTESIAN_POINT('Ctrl Pts',(-31.4703968220572,0.63919516156767,308.193063406947));
#12397=CARTESIAN_POINT('Ctrl Pts',(-31.5072538147313,0.75416812576042,308.20088161175));
#12398=CARTESIAN_POINT('Ctrl Pts',(-31.5175201769259,0.784117020266229,
308.202949667796));
#12399=CARTESIAN_POINT('Ctrl Pts',(-31.5361368121047,0.835076152500721,
308.206527882576));
#12400=CARTESIAN_POINT('Ctrl Pts',(-31.544193850152,0.856189404091126,308.208028156098));
#12401=CARTESIAN_POINT('Ctrl Pts',(-31.5613027667926,0.899168767006922,
308.211120400115));
#12402=CARTESIAN_POINT('Ctrl Pts',(-31.570382662337,0.921020904430828,308.212713180184));
#12403=CARTESIAN_POINT('Ctrl Pts',(-31.5946314300359,0.977000226598203,
308.216848603413));
#12404=CARTESIAN_POINT('Ctrl Pts',(-31.6102816227445,1.01091042292533,308.219407391134));
#12405=CARTESIAN_POINT('Ctrl Pts',(-31.7173305104773,1.2291624155334,308.236238677221));
#12406=CARTESIAN_POINT('Ctrl Pts',(-31.8315760291555,1.40128623380289,308.251334134545));
#12407=CARTESIAN_POINT('Ctrl Pts',(-32.0262345803278,1.62509736453917,308.272926304669));
#12408=CARTESIAN_POINT('Ctrl Pts',(-32.0898228200421,1.69023755513334,308.27948724754));
#12409=CARTESIAN_POINT('Ctrl Pts',(-32.1728514796577,1.76603998074251,308.287325795958));
#12410=CARTESIAN_POINT('Ctrl Pts',(-32.1888976290546,1.78029513519444,308.288809479986));
#12411=CARTESIAN_POINT('Ctrl Pts',(-32.215195335303,1.80302645377075,308.291188046395));
#12412=CARTESIAN_POINT('Ctrl Pts',(-32.2253281891676,1.81163732946813,308.292092123479));
#12413=CARTESIAN_POINT('Ctrl Pts',(-32.2458231096099,1.82875912086157,308.293895033539));
#12414=CARTESIAN_POINT('Ctrl Pts',(-32.2561859809717,1.83726827810096,308.294793740374));
#12415=CARTESIAN_POINT('Ctrl Pts',(-32.2837318206295,1.85949829211333,308.297150505908));
#12416=CARTESIAN_POINT('Ctrl Pts',(-32.3010348300074,1.87306922624968,308.298598432046));
#12417=CARTESIAN_POINT('Ctrl Pts',(-32.400582607225,1.94893343472034,308.306761995695));
#12418=CARTESIAN_POINT('Ctrl Pts',(-32.4866436364809,2.00605563072422,308.313184456185));
#12419=CARTESIAN_POINT('Ctrl Pts',(-32.6070478095626,2.07511031170053,308.32173150813));
#12420=CARTESIAN_POINT('Ctrl Pts',(-32.6383186771404,2.09212059175199,308.323913715546));
#12421=CARTESIAN_POINT('Ctrl Pts',(-32.6699491752354,2.10841545730937,308.326094215555));
#12422=CARTESIAN_POINT('Origin',(-33.7561270252576,0.,302.151410108095));
#12423=CARTESIAN_POINT('',(-32.6699489539077,2.1084153432895,309.521847592916));
#12424=CARTESIAN_POINT('',(-32.6699490796625,2.10841540807375,309.323530658174));
#12425=CARTESIAN_POINT('',(-32.6699490794746,2.10841540797695,302.151410108095));
#12426=CARTESIAN_POINT('',(-36.1278768462125,-0.000921574914906319,308.850490323558));
#12427=CARTESIAN_POINT('Ctrl Pts',(-32.6699489539077,2.1084153432895,309.521847592916));
#12428=CARTESIAN_POINT('Ctrl Pts',(-32.582917846397,2.06358011630052,309.515816690897));
#12429=CARTESIAN_POINT('Ctrl Pts',(-32.498706923478,2.01337899071228,309.509858285855));
#12430=CARTESIAN_POINT('Ctrl Pts',(-32.404470529489,1.94896991467382,309.502811052731));
#12431=CARTESIAN_POINT('Ctrl Pts',(-32.3912276866308,1.93971874165601,309.501811619914));
#12432=CARTESIAN_POINT('Ctrl Pts',(-32.3584887098188,1.91634669603684,309.49931615118));
#12433=CARTESIAN_POINT('Ctrl Pts',(-32.3391113321401,1.90206309192492,309.497816975652));
#12434=CARTESIAN_POINT('Ctrl Pts',(-32.2629535455094,1.84411532160427,309.491826734868));
#12435=CARTESIAN_POINT('Ctrl Pts',(-32.2079506655363,1.79818710465182,309.487277956005));
#12436=CARTESIAN_POINT('Ctrl Pts',(-32.1350754708979,1.73151019749231,309.480868475922));
#12437=CARTESIAN_POINT('Ctrl Pts',(-32.11535460679,1.7128343404082,309.479092660394));
#12438=CARTESIAN_POINT('Ctrl Pts',(-32.0799060995893,1.67809020921673,309.475820547609));
#12439=CARTESIAN_POINT('Ctrl Pts',(-32.0640777482451,1.66212891405747,309.474328988195));
#12440=CARTESIAN_POINT('Ctrl Pts',(-32.0322127436525,1.62906936953523,309.471261400308));
#12441=CARTESIAN_POINT('Ctrl Pts',(-32.0161979822021,1.61195357177694,309.469684661158));
#12442=CARTESIAN_POINT('Ctrl Pts',(-31.9761000379658,1.56780502393637,309.465644563816));
#12443=CARTESIAN_POINT('Ctrl Pts',(-31.9523780890904,1.54045389148599,309.463166481503));
#12444=CARTESIAN_POINT('Ctrl Pts',(-31.8349685195819,1.39865047327097,309.450435618493));
#12445=CARTESIAN_POINT('Ctrl Pts',(-31.7515227476866,1.27617452644095,309.439786669305));
#12446=CARTESIAN_POINT('Ctrl Pts',(-31.6106455816979,1.02112816321664,309.418529871605));
#12447=CARTESIAN_POINT('Ctrl Pts',(-31.5527977401673,0.889460175178401,
309.407978794437));
#12448=CARTESIAN_POINT('Ctrl Pts',(-31.4990984677548,0.729158223731884,
309.396124782373));
#12449=CARTESIAN_POINT('Ctrl Pts',(-31.49138133326,0.704823883845353,309.394351693044));
#12450=CARTESIAN_POINT('Ctrl Pts',(-31.4799988534136,0.666812456690814,
309.391627796626));
#12451=CARTESIAN_POINT('Ctrl Pts',(-31.4760607809486,0.653219912869499,
309.390662759126));
#12452=CARTESIAN_POINT('Ctrl Pts',(-31.468788026443,0.62725006950077,309.388837145454));
#12453=CARTESIAN_POINT('Ctrl Pts',(-31.4654316795447,0.614879813954728,
309.387975475822));
#12454=CARTESIAN_POINT('Ctrl Pts',(-31.4573531918775,0.584120992718638,
309.38585136353));
#12455=CARTESIAN_POINT('Ctrl Pts',(-31.452751123251,0.565701319274591,309.384595566348));
#12456=CARTESIAN_POINT('Ctrl Pts',(-31.4351512027875,0.491479318968117,
309.379592894724));
#12457=CARTESIAN_POINT('Ctrl Pts',(-31.4239550887477,0.435265310580698,
309.375933915341));
#12458=CARTESIAN_POINT('Ctrl Pts',(-31.3963932157845,0.26486172104055,309.365081387851));
#12459=CARTESIAN_POINT('Ctrl Pts',(-31.3863064675317,0.14982963374252,309.358068847602));
#12460=CARTESIAN_POINT('Ctrl Pts',(-31.3826744987209,-0.0997217234533173,
309.342756795197));
#12461=CARTESIAN_POINT('Ctrl Pts',(-31.3921215190607,-0.233865917713545,
309.33445536906));
#12462=CARTESIAN_POINT('Ctrl Pts',(-31.4182392734203,-0.400861272744113,
309.32355316731));
#12463=CARTESIAN_POINT('Ctrl Pts',(-31.4243718042195,-0.43511640447206,
309.321287380491));
#12464=CARTESIAN_POINT('Ctrl Pts',(-31.4358388033042,-0.491932266233717,
309.317473366715));
#12465=CARTESIAN_POINT('Ctrl Pts',(-31.4407545355054,-0.514572596182473,
309.31593860045));
#12466=CARTESIAN_POINT('Ctrl Pts',(-31.4511987445333,-0.55949122248238,
309.312861983124));
#12467=CARTESIAN_POINT('Ctrl Pts',(-31.4567205429137,-0.581768486535565,
309.311320497478));
#12468=CARTESIAN_POINT('Ctrl Pts',(-31.4711326271638,-0.636498825868149,
309.307493059471));
#12469=CARTESIAN_POINT('Ctrl Pts',(-31.4803916634546,-0.668848648627756,
309.305195404129));
#12470=CARTESIAN_POINT('Ctrl Pts',(-31.5238445776484,-0.80930053743524,
309.295059102266));
#12471=CARTESIAN_POINT('Ctrl Pts',(-31.5650721323529,-0.91505416768145,
309.286996661471));
#12472=CARTESIAN_POINT('Ctrl Pts',(-31.6765407858452,-1.14977401429132,
309.268182170353));
#12473=CARTESIAN_POINT('Ctrl Pts',(-31.7515089609208,-1.27599579489191,
309.257363799474));
#12474=CARTESIAN_POINT('Ctrl Pts',(-31.8671769011031,-1.43512675390416,
309.243260663563));
#12475=CARTESIAN_POINT('Ctrl Pts',(-31.8979974935542,-1.47481416408846,
309.239702752355));
#12476=CARTESIAN_POINT('Ctrl Pts',(-31.9419637846782,-1.52786056471875,
309.234921798854));
#12477=CARTESIAN_POINT('Ctrl Pts',(-31.9540394178916,-1.54208510777342,
309.233637176521));
#12478=CARTESIAN_POINT('Ctrl Pts',(-31.9746559028175,-1.56579742707062,
309.231493424462));
#12479=CARTESIAN_POINT('Ctrl Pts',(-31.983107584576,-1.57536124047924,309.23062818555));
#12480=CARTESIAN_POINT('Ctrl Pts',(-32.0011829532596,-1.595485337511,309.22880690146));
#12481=CARTESIAN_POINT('Ctrl Pts',(-32.0108254596443,-1.60602759301231,
309.227852249285));
#12482=CARTESIAN_POINT('Ctrl Pts',(-32.0384107634363,-1.63564502771147,
309.225166456635));
#12483=CARTESIAN_POINT('Ctrl Pts',(-32.0565756312691,-1.654511713786,309.223451036351));
#12484=CARTESIAN_POINT('Ctrl Pts',(-32.1416706961535,-1.74001378523437,
309.215633528912));
#12485=CARTESIAN_POINT('Ctrl Pts',(-32.2122372569251,-1.80292132708271,
309.20975552791));
#12486=CARTESIAN_POINT('Ctrl Pts',(-32.4321362320836,-1.9765471002056,309.192497833265));
#12487=CARTESIAN_POINT('Ctrl Pts',(-32.5908981103255,-2.0741087536459,309.181299310397));
#12488=CARTESIAN_POINT('Ctrl Pts',(-32.7970256599932,-2.16957159527893,
309.166751130648));
#12489=CARTESIAN_POINT('Ctrl Pts',(-32.8350879524938,-2.18600160773769,
309.164067494005));
#12490=CARTESIAN_POINT('Ctrl Pts',(-32.8962828983008,-2.21053511335361,
309.159745472607));
#12491=CARTESIAN_POINT('Ctrl Pts',(-32.9191452966412,-2.21929243695327,
309.158129208124));
#12492=CARTESIAN_POINT('Ctrl Pts',(-32.9630581327344,-2.23533797374362,
309.155019640006));
#12493=CARTESIAN_POINT('Ctrl Pts',(-32.9840837980182,-2.24268663032945,
309.153528554313));
#12494=CARTESIAN_POINT('Ctrl Pts',(-33.0331796659499,-2.25907385531725,
309.150040173177));
#12495=CARTESIAN_POINT('Ctrl Pts',(-33.0613206132316,-2.26788700796187,
309.148035691317));
#12496=CARTESIAN_POINT('Ctrl Pts',(-33.1576495363788,-2.29609406856535,
309.141153906513));
#12497=CARTESIAN_POINT('Ctrl Pts',(-33.2265338182193,-2.31295320593156,
309.136197152153));
#12498=CARTESIAN_POINT('Ctrl Pts',(-33.4101614861645,-2.3492622620895,309.122892671633));
#12499=CARTESIAN_POINT('Ctrl Pts',(-33.5257547656435,-2.36339786748194,
309.114418367836));
#12500=CARTESIAN_POINT('Ctrl Pts',(-33.7581461584435,-2.37460246040821,
309.09742337872));
#12501=CARTESIAN_POINT('Ctrl Pts',(-33.8746497067424,-2.37164454226935,
309.088926563471));
#12502=CARTESIAN_POINT('Ctrl Pts',(-34.0173803038589,-2.35747235492378,
309.078846755644));
#12503=CARTESIAN_POINT('Ctrl Pts',(-34.0442409608706,-2.35434060703294,
309.076964791605));
#12504=CARTESIAN_POINT('Ctrl Pts',(-34.0855324296812,-2.34880902523242,
309.074100660093));
#12505=CARTESIAN_POINT('Ctrl Pts',(-34.1000035358569,-2.34673405636085,
309.073102389376));
#12506=CARTESIAN_POINT('Ctrl Pts',(-34.1269684144957,-2.34261285098788,
309.071253677709));
#12507=CARTESIAN_POINT('Ctrl Pts',(-34.1394657637297,-2.34060029159364,
309.070401594835));
#12508=CARTESIAN_POINT('Ctrl Pts',(-34.1696559622773,-2.33549019773581,
309.068353772767));
#12509=CARTESIAN_POINT('Ctrl Pts',(-34.1873307288394,-2.33229158999825,
309.067163591322));
#12510=CARTESIAN_POINT('Ctrl Pts',(-34.252615775204,-2.31970938051097,309.062793984578));
#12511=CARTESIAN_POINT('Ctrl Pts',(-34.299974193986,-2.30906554334728,309.059676620257));
#12512=CARTESIAN_POINT('Ctrl Pts',(-34.4295782247191,-2.27572759823802,
309.051207415679));
#12513=CARTESIAN_POINT('Ctrl Pts',(-34.5109794380923,-2.25003829031335,
309.045956629941));
#12514=CARTESIAN_POINT('Ctrl Pts',(-34.7464045103643,-2.16152159694816,
309.030528449423));
#12515=CARTESIAN_POINT('Ctrl Pts',(-34.89538899509,-2.08683993033501,309.020413185223));
#12516=CARTESIAN_POINT('Ctrl Pts',(-35.0684907215898,-1.97596801079345,
309.007220618518));
#12517=CARTESIAN_POINT('Ctrl Pts',(-35.1011077888881,-1.95391261525189,
309.004667502444));
#12518=CARTESIAN_POINT('Ctrl Pts',(-35.152754485657,-1.91708346639304,309.000504737959));
#12519=CARTESIAN_POINT('Ctrl Pts',(-35.1721351104655,-1.90281326229172,
308.998914331998));
#12520=CARTESIAN_POINT('Ctrl Pts',(-35.2091363711938,-1.87469040674458,
308.995820618641));
#12521=CARTESIAN_POINT('Ctrl Pts',(-35.2267844550389,-1.86087800379728,
308.994319007283));
#12522=CARTESIAN_POINT('Ctrl Pts',(-35.2679595766136,-1.82770041326181,
308.990751922248));
#12523=CARTESIAN_POINT('Ctrl Pts',(-35.2913138744813,-1.80812821747955,
308.988678232333));
#12524=CARTESIAN_POINT('Ctrl Pts',(-35.3734372298396,-1.73656612640412,
308.981199324187));
#12525=CARTESIAN_POINT('Ctrl Pts',(-35.4299901103301,-1.68212193645288,
308.975694338502));
#12526=CARTESIAN_POINT('Ctrl Pts',(-35.580920113046,-1.52165967802093,308.959970510257));
#12527=CARTESIAN_POINT('Ctrl Pts',(-35.6686330434314,-1.4098342691143,308.949551333526));
#12528=CARTESIAN_POINT('Ctrl Pts',(-35.7952550960688,-1.21466208266615,
308.932614583666));
#12529=CARTESIAN_POINT('Ctrl Pts',(-35.8402755650529,-1.13568282327124,
308.926061119853));
#12530=CARTESIAN_POINT('Ctrl Pts',(-35.890319192324,-1.03484018287382,308.918208815548));
#12531=CARTESIAN_POINT('Ctrl Pts',(-35.8997127471641,-1.01523925635252,
308.916705807547));
#12532=CARTESIAN_POINT('Ctrl Pts',(-35.9144414319581,-0.983389716297388,
308.914304071944));
#12533=CARTESIAN_POINT('Ctrl Pts',(-35.9199446176145,-0.971220809855372,
308.91339584066));
#12534=CARTESIAN_POINT('Ctrl Pts',(-35.9307430585327,-0.946795333458533,
308.911592528836));
#12535=CARTESIAN_POINT('Ctrl Pts',(-35.9360382010261,-0.934539235856524,
308.910697476923));
#12536=CARTESIAN_POINT('Ctrl Pts',(-35.949672660231,-0.902234482642457,
308.908362270637));
#12537=CARTESIAN_POINT('Ctrl Pts',(-35.9578408615002,-0.882114380772325,
308.906931915534));
#12538=CARTESIAN_POINT('Ctrl Pts',(-36.0008941077198,-0.771739135686172,
308.89920082097));
#12539=CARTESIAN_POINT('Ctrl Pts',(-36.0305111005879,-0.679515972858705,
308.89315761057));
#12540=CARTESIAN_POINT('Ctrl Pts',(-36.1031262460622,-0.394589597126578,
308.875018901751));
#12541=CARTESIAN_POINT('Ctrl Pts',(-36.1278002130236,-0.198143471055984,
308.863159774315));
#12542=CARTESIAN_POINT('Ctrl Pts',(-36.1278768462125,-0.000921574914906319,
308.850490323558));
#12543=CARTESIAN_POINT('Ctrl Pts',(-36.1278768471091,-0.000919264543416605,
308.850490175141));
#12544=CARTESIAN_POINT('Ctrl Pts',(-36.1278862217721,0.0232678484348831,
308.848936404638));
#12545=CARTESIAN_POINT('Ctrl Pts',(-36.1275256059454,0.0474531569991235,
308.847372543808));
#12546=CARTESIAN_POINT('Ctrl Pts',(-36.1261053066843,0.0944605704131066,
308.844310220116));
#12547=CARTESIAN_POINT('Ctrl Pts',(-36.1250856458576,0.117281064656113,
308.842813128077));
#12548=CARTESIAN_POINT('Ctrl Pts',(-36.1224986940257,0.161004483537275,
308.839922721874));
#12549=CARTESIAN_POINT('Ctrl Pts',(-36.1209835962592,0.181908408395625,
308.838531160638));
#12550=CARTESIAN_POINT('Ctrl Pts',(-36.117420451444,0.223429120442819,308.835746618048));
#12551=CARTESIAN_POINT('Ctrl Pts',(-36.1153788981696,0.244044604936424,
308.834353960904));
#12552=CARTESIAN_POINT('Ctrl Pts',(-36.1092757530738,0.298402547938392,
308.83065390751));
#12553=CARTESIAN_POINT('Ctrl Pts',(-36.1047586302258,0.33208792654728,308.828332403118));
#12554=CARTESIAN_POINT('Ctrl Pts',(-36.0816687472503,0.480061977446924,
308.818002625462));
#12555=CARTESIAN_POINT('Ctrl Pts',(-36.0554676865038,0.592983419147006,
308.809760530729));
#12556=CARTESIAN_POINT('Ctrl Pts',(-36.0025918769121,0.763217153179421,
308.796842910466));
#12557=CARTESIAN_POINT('Ctrl Pts',(-35.9816997077517,0.822150002649554,
308.79227828608));
#12558=CARTESIAN_POINT('Ctrl Pts',(-35.9271683739195,0.958596643332158,
308.781545072691));
#12559=CARTESIAN_POINT('Ctrl Pts',(-35.8916653789878,1.03528032714506,308.775382073959));
#12560=CARTESIAN_POINT('Ctrl Pts',(-35.8295735041397,1.15253826726458,308.765887137372));
#12561=CARTESIAN_POINT('Ctrl Pts',(-35.8057035077327,1.19447131913051,308.762477090076));
#12562=CARTESIAN_POINT('Ctrl Pts',(-35.7712314522354,1.25094902406481,308.757892123523));
#12563=CARTESIAN_POINT('Ctrl Pts',(-35.7617200882782,1.26614210407465,308.756659550395));
#12564=CARTESIAN_POINT('Ctrl Pts',(-35.7452018132878,1.29187447156993,308.754575295973));
#12565=CARTESIAN_POINT('Ctrl Pts',(-35.7382813044423,1.30246789090213,308.753718294113));
#12566=CARTESIAN_POINT('Ctrl Pts',(-35.7231722884601,1.32519631123206,308.751882307876));
#12567=CARTESIAN_POINT('Ctrl Pts',(-35.7149557654274,1.33731160380046,308.750905162207));
#12568=CARTESIAN_POINT('Ctrl Pts',(-35.6911909858697,1.37166384344761,308.748136478314));
#12569=CARTESIAN_POINT('Ctrl Pts',(-35.6753720793933,1.3937118805038,308.746361844236));
#12570=CARTESIAN_POINT('Ctrl Pts',(-35.5352506319563,1.58209836200981,308.731173211207));
#12571=CARTESIAN_POINT('Ctrl Pts',(-35.3899655465321,1.73173651632426,308.718867317132));
#12572=CARTESIAN_POINT('Ctrl Pts',(-35.1562189710855,1.91653027403662,308.700373004404));
#12573=CARTESIAN_POINT('Ctrl Pts',(-35.0822787592643,1.96841680140534,308.694686884142));
#12574=CARTESIAN_POINT('Ctrl Pts',(-34.9785567855332,2.03270099909018,308.686786311959));
#12575=CARTESIAN_POINT('Ctrl Pts',(-34.9512136998376,2.04889617916726,308.684710710447));
#12576=CARTESIAN_POINT('Ctrl Pts',(-34.9038651896521,2.07567020437022,308.681123539355));
#12577=CARTESIAN_POINT('Ctrl Pts',(-34.8840181907516,2.08652130346246,308.679621985114));
#12578=CARTESIAN_POINT('Ctrl Pts',(-34.8456201485913,2.10680702098609,308.67671931056));
#12579=CARTESIAN_POINT('Ctrl Pts',(-34.8270940940707,2.11628461671639,308.675319892015));
#12580=CARTESIAN_POINT('Ctrl Pts',(-34.7774980254699,2.14083906466294,308.671575000399));
#12581=CARTESIAN_POINT('Ctrl Pts',(-34.7462203805165,2.15548267205838,308.669214764579));
#12582=CARTESIAN_POINT('Ctrl Pts',(-34.5984720496493,2.22076136003469,308.658066403211));
#12583=CARTESIAN_POINT('Ctrl Pts',(-34.4783919752916,2.26266447026487,308.648992181369));
#12584=CARTESIAN_POINT('Ctrl Pts',(-34.2381554635698,2.3254180618445,308.630947206709));
#12585=CARTESIAN_POINT('Ctrl Pts',(-34.118578437241,2.34703003429443,308.622018407052));
#12586=CARTESIAN_POINT('Ctrl Pts',(-33.9394147706663,2.36538724422373,308.60905228964));
#12587=CARTESIAN_POINT('Ctrl Pts',(-33.8807495393507,2.36920274653735,308.60487347458));
#12588=CARTESIAN_POINT('Ctrl Pts',(-33.8028682399745,2.37136660309827,308.599462337036));
#12589=CARTESIAN_POINT('Ctrl Pts',(-33.7837315743911,2.37166657772787,308.598143676686));
#12590=CARTESIAN_POINT('Ctrl Pts',(-33.7517494603085,2.37178073355751,308.595960428266));
#12591=CARTESIAN_POINT('Ctrl Pts',(-33.7389056297561,2.37172225759975,308.595089213291));
#12592=CARTESIAN_POINT('Ctrl Pts',(-33.7119721109922,2.37138081452743,308.593274668689));
#12593=CARTESIAN_POINT('Ctrl Pts',(-33.6978834797453,2.37107662018926,308.592332473324));
#12594=CARTESIAN_POINT('Ctrl Pts',(-33.6585729303756,2.36987724468739,308.58972089853));
#12595=CARTESIAN_POINT('Ctrl Pts',(-33.6333605530284,2.36870502073593,308.588065889776));
#12596=CARTESIAN_POINT('Ctrl Pts',(-33.4614682681724,2.35796096139347,308.576889349087));
#12597=CARTESIAN_POINT('Ctrl Pts',(-33.3159165514741,2.33517228013113,308.567943942551));
#12598=CARTESIAN_POINT('Ctrl Pts',(-33.0779989715817,2.27486831545843,308.552901597502));
#12599=CARTESIAN_POINT('Ctrl Pts',(-32.9842027180859,2.24477497530487,308.546858397503));
#12600=CARTESIAN_POINT('Ctrl Pts',(-32.851053115634,2.1927208227923,308.537864870895));
#12601=CARTESIAN_POINT('Ctrl Pts',(-32.8100221092461,2.17533181889552,308.535034369012));
#12602=CARTESIAN_POINT('Ctrl Pts',(-32.7359475555572,2.14144666423182,308.529794219967));
#12603=CARTESIAN_POINT('Ctrl Pts',(-32.7027526725709,2.12531461068094,308.527396545889));
#12604=CARTESIAN_POINT('Ctrl Pts',(-32.6699490794745,2.10841540797688,308.52497223169));
#12605=CARTESIAN_POINT('Ctrl Pts',(-32.6699491752354,2.10841545730937,308.326094215555));
#12606=CARTESIAN_POINT('Ctrl Pts',(-32.755914322101,2.15270152914386,308.332020363251));
#12607=CARTESIAN_POINT('Ctrl Pts',(-32.8445355875257,2.19170323357068,308.337937841171));
#12608=CARTESIAN_POINT('Ctrl Pts',(-33.0065151287818,2.25145240174275,308.348726318251));
#12609=CARTESIAN_POINT('Ctrl Pts',(-33.0789197856405,2.27427891086674,308.353538732903));
#12610=CARTESIAN_POINT('Ctrl Pts',(-33.1814425011099,2.30127021402803,308.360418141556));
#12611=CARTESIAN_POINT('Ctrl Pts',(-33.2107385563569,2.30838865496917,308.362390941712));
#12612=CARTESIAN_POINT('Ctrl Pts',(-33.2619872288921,2.31981119091254,308.365858417377));
#12613=CARTESIAN_POINT('Ctrl Pts',(-33.2838802262251,2.3243667959624,308.367344834049));
#12614=CARTESIAN_POINT('Ctrl Pts',(-33.3295847869115,2.33320487479391,308.370460193041));
#12615=CARTESIAN_POINT('Ctrl Pts',(-33.353403909653,2.33743391038815,308.372090655622));
#12616=CARTESIAN_POINT('Ctrl Pts',(-33.4167673669361,2.34768671985371,308.376448084637));
#12617=CARTESIAN_POINT('Ctrl Pts',(-33.4564049945613,2.35307549354416,308.379194668971));
#12618=CARTESIAN_POINT('Ctrl Pts',(-33.6526684499597,2.37471847086801,308.392903945151));
#12619=CARTESIAN_POINT('Ctrl Pts',(-33.8104844659483,2.37634626975723,308.404308686156));
#12620=CARTESIAN_POINT('Ctrl Pts',(-34.0575130415806,2.35426703884362,308.422423511865));
#12621=CARTESIAN_POINT('Ctrl Pts',(-34.1472230007346,2.34103655628998,308.429048221489));
#12622=CARTESIAN_POINT('Ctrl Pts',(-34.2851867169996,2.31253555044959,308.439142452669));
#12623=CARTESIAN_POINT('Ctrl Pts',(-34.3340825891992,2.30080268812649,308.442700371206));
#12624=CARTESIAN_POINT('Ctrl Pts',(-34.4001058222401,2.2827220270776,308.447446213859));
#12625=CARTESIAN_POINT('Ctrl Pts',(-34.4175842939109,2.27771878802323,308.448696914189));
#12626=CARTESIAN_POINT('Ctrl Pts',(-34.4471614941797,2.26888307666137,308.450801698355));
#12627=CARTESIAN_POINT('Ctrl Pts',(-34.4592898474382,2.26515366580934,308.451661377836));
#12628=CARTESIAN_POINT('Ctrl Pts',(-34.4852184255709,2.25695241315396,308.453491388417));
#12629=CARTESIAN_POINT('Ctrl Pts',(-34.4990083913671,2.25245105798967,308.45446004502));
#12630=CARTESIAN_POINT('Ctrl Pts',(-34.5378785432566,2.23936715245333,308.457179628251));
#12631=CARTESIAN_POINT('Ctrl Pts',(-34.5628582088819,2.23048999547421,308.458914566906));
#12632=CARTESIAN_POINT('Ctrl Pts',(-34.6812408198761,2.18617061385757,308.467099168501));
#12633=CARTESIAN_POINT('Ctrl Pts',(-34.7725006788235,2.14526602339269,308.473298485368));
#12634=CARTESIAN_POINT('Ctrl Pts',(-34.9746165308118,2.03887012752612,308.487346527652));
#12635=CARTESIAN_POINT('Ctrl Pts',(-35.083260673448,1.96987899931533,308.495144083049));
#12636=CARTESIAN_POINT('Ctrl Pts',(-35.245421458766,1.84737304581892,308.507851467831));
#12637=CARTESIAN_POINT('Ctrl Pts',(-35.3028935556564,1.79952681061178,308.512594610753));
#12638=CARTESIAN_POINT('Ctrl Pts',(-35.3801318217029,1.72878759963456,308.51939242449));
#12639=CARTESIAN_POINT('Ctrl Pts',(-35.4018690274413,1.70810751176898,308.521356044168));
#12640=CARTESIAN_POINT('Ctrl Pts',(-35.4390982939029,1.67131830645251,308.524812996333));
#12641=CARTESIAN_POINT('Ctrl Pts',(-35.4547660930301,1.65539192691172,308.526298224071));
#12642=CARTESIAN_POINT('Ctrl Pts',(-35.4869673900299,1.62172063234602,308.529416591302));
#12643=CARTESIAN_POINT('Ctrl Pts',(-35.503458288442,1.60393876387111,308.531051326935));
#12644=CARTESIAN_POINT('Ctrl Pts',(-35.5466199436454,1.55594254872147,308.53543396001));
#12645=CARTESIAN_POINT('Ctrl Pts',(-35.5727971433412,1.52529716513599,308.538201885445));
#12646=CARTESIAN_POINT('Ctrl Pts',(-35.6852502820034,1.3866462902974,308.55060044161));
#12647=CARTESIAN_POINT('Ctrl Pts',(-35.7627564181842,1.27190105467278,308.560559329088));
#12648=CARTESIAN_POINT('Ctrl Pts',(-35.8803492441535,1.06005491438619,308.578232819097));
#12649=CARTESIAN_POINT('Ctrl Pts',(-35.9248289450757,0.965800034558325,
308.585870026231));
#12650=CARTESIAN_POINT('Ctrl Pts',(-35.9828715558642,0.818386804260248,
308.597248914254));
#12651=CARTESIAN_POINT('Ctrl Pts',(-36.0010304084179,0.767175312144135,
308.601102179311));
#12652=CARTESIAN_POINT('Ctrl Pts',(-36.0230435467245,0.697592755418938,
308.606166492897));
#12653=CARTESIAN_POINT('Ctrl Pts',(-36.0284612842857,0.679737624759728,
308.607451114757));
#12654=CARTESIAN_POINT('Ctrl Pts',(-36.0372290353312,0.649564888446928,
308.609594819222));
#12655=CARTESIAN_POINT('Ctrl Pts',(-36.0406912728289,0.637281064922245,
308.61046001159));
#12656=CARTESIAN_POINT('Ctrl Pts',(-36.047818419668,0.611189545029289,308.612281131709));
#12657=CARTESIAN_POINT('Ctrl Pts',(-36.0514580015008,0.597375797176231,
308.61323566757));
#12658=CARTESIAN_POINT('Ctrl Pts',(-36.0614141046315,0.558153201248831,
308.615920973423));
#12659=CARTESIAN_POINT('Ctrl Pts',(-36.0674352388617,0.532670625336184,
308.617636030936));
#12660=CARTESIAN_POINT('Ctrl Pts',(-36.109333487345,0.341237385765275,308.630335671899));
#12661=CARTESIAN_POINT('Ctrl Pts',(-36.1277245328718,0.171942280673287,
308.640560893311));
#12662=CARTESIAN_POINT('Ctrl Pts',(-36.1279869436714,-0.122117100655979,
308.658629064496));
#12663=CARTESIAN_POINT('Ctrl Pts',(-36.1183368969789,-0.246153070808098,
308.666341823443));
#12664=CARTESIAN_POINT('Ctrl Pts',(-36.0936659959656,-0.402857955791089,
308.676578386888));
#12665=CARTESIAN_POINT('Ctrl Pts',(-36.0875732146422,-0.436739556674402,
308.678820596967));
#12666=CARTESIAN_POINT('Ctrl Pts',(-36.0766216258432,-0.49085136791343,
308.682454397209));
#12667=CARTESIAN_POINT('Ctrl Pts',(-36.0722301204751,-0.511171852239556,
308.683831029533));
#12668=CARTESIAN_POINT('Ctrl Pts',(-36.0625009395971,-0.553488632726168,
308.686724420006));
#12669=CARTESIAN_POINT('Ctrl Pts',(-36.0571143997941,-0.575471406683232,
308.688242623345));
#12670=CARTESIAN_POINT('Ctrl Pts',(-36.0433885791615,-0.628210141620436,
308.691923089821));
#12671=CARTESIAN_POINT('Ctrl Pts',(-36.0347426417342,-0.658880943506679,
308.694095068142));
#12672=CARTESIAN_POINT('Ctrl Pts',(-35.9989869521985,-0.776586526600283,
308.702557309091));
#12673=CARTESIAN_POINT('Ctrl Pts',(-35.9674892081753,-0.862195433089648,
308.70898655651));
#12674=CARTESIAN_POINT('Ctrl Pts',(-35.8901584996685,-1.04003537782102,
308.722913369648));
#12675=CARTESIAN_POINT('Ctrl Pts',(-35.843086591684,-1.13153059083709,308.730429265905));
#12676=CARTESIAN_POINT('Ctrl Pts',(-35.7365967528101,-1.3091278227897,308.745548590452));
#12677=CARTESIAN_POINT('Ctrl Pts',(-35.6771147853955,-1.394950124037,308.753135071191));
#12678=CARTESIAN_POINT('Ctrl Pts',(-35.5955486732657,-1.49747751579554,
308.762338456356));
#12679=CARTESIAN_POINT('Ctrl Pts',(-35.5785740111191,-1.51809026146944,
308.764196117664));
#12680=CARTESIAN_POINT('Ctrl Pts',(-35.5518189085454,-1.54948388460021,
308.767031284715));
#12681=CARTESIAN_POINT('Ctrl Pts',(-35.5422818287423,-1.56046810101882,
308.768024420975));
#12682=CARTESIAN_POINT('Ctrl Pts',(-35.524244995528,-1.58085977046966,308.769869161196));
#12683=CARTESIAN_POINT('Ctrl Pts',(-35.5157703858732,-1.59028740222343,
308.770722320216));
#12684=CARTESIAN_POINT('Ctrl Pts',(-35.495014037886,-1.61300884614629,308.772780140531));
#12685=CARTESIAN_POINT('Ctrl Pts',(-35.482655050401,-1.62623079824287,308.77397909457));
#12686=CARTESIAN_POINT('Ctrl Pts',(-35.4358558556527,-1.67516276255752,
308.77842774005));
#12687=CARTESIAN_POINT('Ctrl Pts',(-35.4004470253281,-1.70993325723489,
308.781612404327));
#12688=CARTESIAN_POINT('Ctrl Pts',(-35.2988615960832,-1.80361088509888,
308.790349975863));
#12689=CARTESIAN_POINT('Ctrl Pts',(-35.2304360908608,-1.85996154405366,
308.795793965617));
#12690=CARTESIAN_POINT('Ctrl Pts',(-35.0294517869233,-2.00740194211723,
308.811077296235));
#12691=CARTESIAN_POINT('Ctrl Pts',(-34.8905789479158,-2.08902634527165,
308.820874153435));
#12692=CARTESIAN_POINT('Ctrl Pts',(-34.7083399199553,-2.17257300130964,
308.833734448743));
#12693=CARTESIAN_POINT('Ctrl Pts',(-34.6717421027349,-2.1882485176744,308.836315124534));
#12694=CARTESIAN_POINT('Ctrl Pts',(-34.61233394576,-2.21194284716722,308.840511423306));
#12695=CARTESIAN_POINT('Ctrl Pts',(-34.5897644520763,-2.22054723390368,
308.842107208608));
#12696=CARTESIAN_POINT('Ctrl Pts',(-34.5460416480166,-2.2364555874454,308.845203768806));
#12697=CARTESIAN_POINT('Ctrl Pts',(-34.5249085689044,-2.24380783147271,
308.846702733638));
#12698=CARTESIAN_POINT('Ctrl Pts',(-34.4749761263737,-2.26039123171864,
308.850251268059));
#12699=CARTESIAN_POINT('Ctrl Pts',(-34.44609856306,-2.26937252999342,308.852308813145));
#12700=CARTESIAN_POINT('Ctrl Pts',(-34.3434722823088,-2.29915080363941,
308.859643289767));
#12701=CARTESIAN_POINT('Ctrl Pts',(-34.2689025740789,-2.31692207183345,
308.865014844814));
#12702=CARTESIAN_POINT('Ctrl Pts',(-34.0699607968685,-2.35425872994888,
308.879448555513));
#12703=CARTESIAN_POINT('Ctrl Pts',(-33.9446694115968,-2.36758795579718,
308.888652647635));
#12704=CARTESIAN_POINT('Ctrl Pts',(-33.7188652186595,-2.37356872371103,
308.905139207028));
#12705=CARTESIAN_POINT('Ctrl Pts',(-33.6187293363754,-2.36988235198688,
308.912409854883));
#12706=CARTESIAN_POINT('Ctrl Pts',(-33.4927374355844,-2.3572286611839,308.921302908025));
#12707=CARTESIAN_POINT('Ctrl Pts',(-33.4664013695178,-2.35413683277247,
308.923147310719));
#12708=CARTESIAN_POINT('Ctrl Pts',(-33.4257440073174,-2.34867102171589,
308.925966683547));
#12709=CARTESIAN_POINT('Ctrl Pts',(-33.4113842059485,-2.34660625650908,
308.926957028393));
#12710=CARTESIAN_POINT('Ctrl Pts',(-33.3845016491944,-2.34248877007525,
308.92879969821));
#12711=CARTESIAN_POINT('Ctrl Pts',(-33.3719756757744,-2.34046721963082,
308.929653530175));
#12712=CARTESIAN_POINT('Ctrl Pts',(-33.3415454546462,-2.33530523906998,
308.931717159824));
#12713=CARTESIAN_POINT('Ctrl Pts',(-33.3236600595272,-2.33205935018824,
308.932921164455));
#12714=CARTESIAN_POINT('Ctrl Pts',(-33.2564835946808,-2.31906854220859,
308.937415846191));
#12715=CARTESIAN_POINT('Ctrl Pts',(-33.207465673826,-2.3079631694293,308.94063973599));
#12716=CARTESIAN_POINT('Ctrl Pts',(-33.0712250235661,-2.27251014506578,
308.949536773535));
#12717=CARTESIAN_POINT('Ctrl Pts',(-32.9849876004306,-2.24471360381062,
308.955096193031));
#12718=CARTESIAN_POINT('Ctrl Pts',(-32.7535954585549,-2.15521541119179,
308.970304752048));
#12719=CARTESIAN_POINT('Ctrl Pts',(-32.612689460885,-2.08388275956713,308.979921139783));
#12720=CARTESIAN_POINT('Ctrl Pts',(-32.4461915820827,-1.97759113447858,
308.992590229454));
#12721=CARTESIAN_POINT('Ctrl Pts',(-32.4130329258623,-1.95522262136585,
308.99518247027));
#12722=CARTESIAN_POINT('Ctrl Pts',(-32.3607517904557,-1.91799665832472,
308.999392876521));
#12723=CARTESIAN_POINT('Ctrl Pts',(-32.3412629222271,-1.90366560204967,
309.000990952808));
#12724=CARTESIAN_POINT('Ctrl Pts',(-32.3041866217484,-1.87551784264914,
309.004088845338));
#12725=CARTESIAN_POINT('Ctrl Pts',(-32.2865686646804,-1.86174549253468,
309.005586804461));
#12726=CARTESIAN_POINT('Ctrl Pts',(-32.2456607655036,-1.82882440575581,
309.009127987267));
#12727=CARTESIAN_POINT('Ctrl Pts',(-32.2225364958187,-1.80947698812294,
309.011179090235));
#12728=CARTESIAN_POINT('Ctrl Pts',(-32.1425164137073,-1.73989062023005,
309.01845670784));
#12729=CARTESIAN_POINT('Ctrl Pts',(-32.0876742642693,-1.68737126940459,
309.023775860508));
#12730=CARTESIAN_POINT('Ctrl Pts',(-31.9442990663464,-1.53623492793395,
309.038625039011));
#12731=CARTESIAN_POINT('Ctrl Pts',(-31.8613642150596,-1.43269210616283,
309.048326108341));
#12732=CARTESIAN_POINT('Ctrl Pts',(-31.730012592139,-1.23720934648075,309.06550529934));
#12733=CARTESIAN_POINT('Ctrl Pts',(-31.6781484869623,-1.14797047469972,
309.07297686459));
#12734=CARTESIAN_POINT('Ctrl Pts',(-31.622466512533,-1.03594128383417,309.081706291512));
#12735=CARTESIAN_POINT('Ctrl Pts',(-31.6129538847782,-1.01611539922906,
309.083227379392));
#12736=CARTESIAN_POINT('Ctrl Pts',(-31.5980864155893,-0.983991140975836,
309.085650720084));
#12737=CARTESIAN_POINT('Ctrl Pts',(-31.5925580023527,-0.97177515097817,
309.086562771749));
#12738=CARTESIAN_POINT('Ctrl Pts',(-31.5817539469891,-0.947352408465521,
309.088366424335));
#12739=CARTESIAN_POINT('Ctrl Pts',(-31.5764767853174,-0.93514689788185,
309.089258081777));
#12740=CARTESIAN_POINT('Ctrl Pts',(-31.5629511307058,-0.903126885636739,
309.091573551144));
#12741=CARTESIAN_POINT('Ctrl Pts',(-31.5548682273033,-0.883243149365324,
309.09298786618));
#12742=CARTESIAN_POINT('Ctrl Pts',(-31.5139528442966,-0.778540198584335,
309.10032657504));
#12743=CARTESIAN_POINT('Ctrl Pts',(-31.4857458779241,-0.691984869993243,
309.106023944894));
#12744=CARTESIAN_POINT('Ctrl Pts',(-31.41018886941,-0.405081611302546,309.124360917937));
#12745=CARTESIAN_POINT('Ctrl Pts',(-31.3839053947335,-0.200195316159489,
309.13669300718));
#12746=CARTESIAN_POINT('Ctrl Pts',(-31.3844702155783,0.0428572830394322,
309.152324877307));
#12747=CARTESIAN_POINT('Ctrl Pts',(-31.3854390539761,0.0801939125581355,
309.154750919709));
#12748=CARTESIAN_POINT('Ctrl Pts',(-31.3884611229818,0.141124724174767,
309.158758888039));
#12749=CARTESIAN_POINT('Ctrl Pts',(-31.3899869402004,0.164739315477346,
309.160324218774));
#12750=CARTESIAN_POINT('Ctrl Pts',(-31.393660131062,0.210852774566611,309.163406315914));
#12751=CARTESIAN_POINT('Ctrl Pts',(-31.3957762725766,0.233351626760168,
309.164921936481));
#12752=CARTESIAN_POINT('Ctrl Pts',(-31.4016279917619,0.287288205038647,
309.168585413533));
#12753=CARTESIAN_POINT('Ctrl Pts',(-31.4056720857848,0.318687338442184,
309.170742759238));
#12754=CARTESIAN_POINT('Ctrl Pts',(-31.4234890987241,0.438102982988947,
309.179045944625));
#12755=CARTESIAN_POINT('Ctrl Pts',(-31.4415869102768,0.525389936095793,
309.185323921831));
#12756=CARTESIAN_POINT('Ctrl Pts',(-31.5155473352017,0.802580054170454,
309.205907855014));
#12757=CARTESIAN_POINT('Ctrl Pts',(-31.5902538657047,0.986569568588838,
309.220645267947));
#12758=CARTESIAN_POINT('Ctrl Pts',(-31.7038788840297,1.18940258691148,309.237108940261));
#12759=CARTESIAN_POINT('Ctrl Pts',(-31.7214920819501,1.21928745545428,309.239538216271));
#12760=CARTESIAN_POINT('Ctrl Pts',(-31.7481213687615,1.26228515095993,309.243027246618));
#12761=CARTESIAN_POINT('Ctrl Pts',(-31.7566230287568,1.27570934090378,309.244115640839));
#12762=CARTESIAN_POINT('Ctrl Pts',(-31.7720554332601,1.29954389762906,309.246045040158));
#12763=CARTESIAN_POINT('Ctrl Pts',(-31.778934372778,1.30998612840426,309.246889156785));
#12764=CARTESIAN_POINT('Ctrl Pts',(-31.7948918446053,1.33379748643985,309.248811488785));
#12765=CARTESIAN_POINT('Ctrl Pts',(-31.8040248426327,1.34712890034042,309.249886108115));
#12766=CARTESIAN_POINT('Ctrl Pts',(-31.8340965072962,1.39007632419035,309.253346307005));
#12767=CARTESIAN_POINT('Ctrl Pts',(-31.8555794189489,1.41930709614109,309.255698722066));
#12768=CARTESIAN_POINT('Ctrl Pts',(-31.9922506111046,1.59659788922086,309.270028442402));
#12769=CARTESIAN_POINT('Ctrl Pts',(-32.1240057784157,1.73106326631051,309.28121503426));
#12770=CARTESIAN_POINT('Ctrl Pts',(-32.282649683095,1.85857901681812,309.293822207718));
#12771=CARTESIAN_POINT('Ctrl Pts',(-32.2951564162165,1.86842615819068,309.294810559461));
#12772=CARTESIAN_POINT('Ctrl Pts',(-32.3721397861375,1.92779324118059,309.300864819143));
#12773=CARTESIAN_POINT('Ctrl Pts',(-32.4390226271458,1.97409256572256,309.306002727732));
#12774=CARTESIAN_POINT('Ctrl Pts',(-32.5349622722325,2.03345744506234,309.313309597567));
#12775=CARTESIAN_POINT('Ctrl Pts',(-32.5621060663155,2.04951368137794,309.315369929092));
#12776=CARTESIAN_POINT('Ctrl Pts',(-32.6090239533855,2.07601837801412,309.318924330877));
#12777=CARTESIAN_POINT('Ctrl Pts',(-32.628640892351,2.08673733977612,309.320408456484));
#12778=CARTESIAN_POINT('Ctrl Pts',(-32.6555678616768,2.10096006507135,309.322443973274));
#12779=CARTESIAN_POINT('Ctrl Pts',(-32.6627490318879,2.10470620870534,309.322986666663));
#12780=CARTESIAN_POINT('Ctrl Pts',(-32.6699490796625,2.10841540807375,309.323530658174));
#12781=CARTESIAN_POINT('Origin',(-33.7561270252576,0.,302.151410108095));
#12782=CARTESIAN_POINT('',(-32.6699490276577,2.10841538128279,310.521403445152));
#12783=CARTESIAN_POINT('',(-32.6699491957805,2.10841546789345,310.326187962698));
#12784=CARTESIAN_POINT('',(-32.6699490794746,2.10841540797695,302.151410108095));
#12785=CARTESIAN_POINT('Ctrl Pts',(-32.6699490276577,2.10841538128279,310.521403445152));
#12786=CARTESIAN_POINT('Ctrl Pts',(-32.617780915958,2.081540290346,310.517169465957));
#12787=CARTESIAN_POINT('Ctrl Pts',(-32.5666123539571,2.05273010432393,310.51298201885));
#12788=CARTESIAN_POINT('Ctrl Pts',(-32.4979212472925,2.01062024751867,310.507361136708));
#12789=CARTESIAN_POINT('Ctrl Pts',(-32.4794493984791,1.99894219094549,310.50584972901));
#12790=CARTESIAN_POINT('Ctrl Pts',(-32.4499314133711,1.97970455000854,310.503437935968));
#12791=CARTESIAN_POINT('Ctrl Pts',(-32.4387837130318,1.97230416058991,310.502527910406));
#12792=CARTESIAN_POINT('Ctrl Pts',(-32.4166595225342,1.95734576613111,310.500724403869));
#12793=CARTESIAN_POINT('Ctrl Pts',(-32.4056829259026,1.94978880766032,310.499830912042));
#12794=CARTESIAN_POINT('Ctrl Pts',(-32.3770857407382,1.92974340384591,310.497504849177));
#12795=CARTESIAN_POINT('Ctrl Pts',(-32.3595705563464,1.91710578218941,310.496081936501));
#12796=CARTESIAN_POINT('Ctrl Pts',(-32.2718341734271,1.85196121953167,310.488949619804));
#12797=CARTESIAN_POINT('Ctrl Pts',(-32.204383184779,1.79582294601288,310.483449646956));
#12798=CARTESIAN_POINT('Ctrl Pts',(-32.0344935085815,1.63768951961566,310.469090477362));
#12799=CARTESIAN_POINT('Ctrl Pts',(-31.9380037174788,1.52986176405891,310.460373753602));
#12800=CARTESIAN_POINT('Ctrl Pts',(-31.8047547888782,1.35040866805719,310.446429939693));
#12801=CARTESIAN_POINT('Ctrl Pts',(-31.7608022339661,1.28457551727009,310.441420304982));
#12802=CARTESIAN_POINT('Ctrl Pts',(-31.7045524684001,1.19045081722967,310.434309054721));
#12803=CARTESIAN_POINT('Ctrl Pts',(-31.689389946886,1.16392827029874,310.432310892572));
#12804=CARTESIAN_POINT('Ctrl Pts',(-31.6639942893277,1.11744415155062,310.428814106828));
#12805=CARTESIAN_POINT('Ctrl Pts',(-31.653524015766,1.09761620895728,310.427324168857));
#12806=CARTESIAN_POINT('Ctrl Pts',(-31.6324151246718,1.05623084753417,310.424216064531));
#12807=CARTESIAN_POINT('Ctrl Pts',(-31.6218200309869,1.03465425145406,310.422596578696));
#12808=CARTESIAN_POINT('Ctrl Pts',(-31.5948051394383,0.977457907023186,
310.418304192467));
#12809=CARTESIAN_POINT('Ctrl Pts',(-31.5789383935358,0.941586744168151,
310.415612719643));
#12810=CARTESIAN_POINT('Ctrl Pts',(-31.4999109302933,0.750232567186608,
310.401249844646));
#12811=CARTESIAN_POINT('Ctrl Pts',(-31.4525059583483,0.588788427757955,
310.389065074152));
#12812=CARTESIAN_POINT('Ctrl Pts',(-31.4074573577671,0.340691815975887,
310.370646577878));
#12813=CARTESIAN_POINT('Ctrl Pts',(-31.3968220638381,0.256907712542552,
310.36448710201));
#12814=CARTESIAN_POINT('Ctrl Pts',(-31.3882549757538,0.13958673197959,310.356069232012));
#12815=CARTESIAN_POINT('Ctrl Pts',(-31.3865314368517,0.106392994363063,
310.353710832094));
#12816=CARTESIAN_POINT('Ctrl Pts',(-31.3847186964737,0.0476642880044788,
310.349590938743));
#12817=CARTESIAN_POINT('Ctrl Pts',(-31.38434307016,0.022143813624543,310.347818238616));
#12818=CARTESIAN_POINT('Ctrl Pts',(-31.384399591134,-0.0175286482664451,
310.345094803976));
#12819=CARTESIAN_POINT('Ctrl Pts',(-31.3845463736195,-0.031678289113071,
310.34412984637));
#12820=CARTESIAN_POINT('Ctrl Pts',(-31.3850646141794,-0.0584949798600393,
310.34231420799));
#12821=CARTESIAN_POINT('Ctrl Pts',(-31.3854109611377,-0.0711615784911806,
310.341462298766));
#12822=CARTESIAN_POINT('Ctrl Pts',(-31.3864178424604,-0.0996325236566917,
310.339559207885));
#12823=CARTESIAN_POINT('Ctrl Pts',(-31.3871350129761,-0.115434527747098,
310.33851106161));
#12824=CARTESIAN_POINT('Ctrl Pts',(-31.3898283746748,-0.164038186627979,
310.335308886666));
#12825=CARTESIAN_POINT('Ctrl Pts',(-31.392328262113,-0.196808244752479,
310.333180322093));
#12826=CARTESIAN_POINT('Ctrl Pts',(-31.4144484664309,-0.424317445746433,
310.318548859895));
#12827=CARTESIAN_POINT('Ctrl Pts',(-31.4574288397828,-0.616041280208117,
310.306910859396));
#12828=CARTESIAN_POINT('Ctrl Pts',(-31.5534541068269,-0.883921612430742,
310.289237425773));
#12829=CARTESIAN_POINT('Ctrl Pts',(-31.5880913327436,-0.965766077800881,
310.283639208161));
#12830=CARTESIAN_POINT('Ctrl Pts',(-31.6411756006865,-1.07386172696808,
310.275840741928));
#12831=CARTESIAN_POINT('Ctrl Pts',(-31.6556842466148,-1.10197028766911,
310.273774418547));
#12832=CARTESIAN_POINT('Ctrl Pts',(-31.6815129759689,-1.14964565064975,
310.27019815604));
#12833=CARTESIAN_POINT('Ctrl Pts',(-31.6925588526082,-1.1693566232149,310.268698070947));
#12834=CARTESIAN_POINT('Ctrl Pts',(-31.7157514323762,-1.20939073344391,
310.26560526524));
#12835=CARTESIAN_POINT('Ctrl Pts',(-31.7279241776211,-1.22969575271207,
310.264011722006));
#12836=CARTESIAN_POINT('Ctrl Pts',(-31.7601028662256,-1.28159425467662,
310.259872166975));
#12837=CARTESIAN_POINT('Ctrl Pts',(-31.7805550331742,-1.31290186374438,
310.25730995041));
#12838=CARTESIAN_POINT('Ctrl Pts',(-31.918175971827,-1.51306752384813,310.240490268461));
#12839=CARTESIAN_POINT('Ctrl Pts',(-32.0561170340056,-1.66654484642878,
310.22541216027));
#12840=CARTESIAN_POINT('Ctrl Pts',(-32.28118636391,-1.8595809317406,310.203827328488));
#12841=CARTESIAN_POINT('Ctrl Pts',(-32.3536758489939,-1.91484341022577,
310.197257402625));
#12842=CARTESIAN_POINT('Ctrl Pts',(-32.4469648231921,-1.97781527856887,
310.189409940672));
#12843=CARTESIAN_POINT('Ctrl Pts',(-32.4649216413154,-1.989584802377,310.187925793156));
#12844=CARTESIAN_POINT('Ctrl Pts',(-32.4942570836578,-2.00824778589239,
310.185546630712));
#12845=CARTESIAN_POINT('Ctrl Pts',(-32.5055378137275,-2.01529193096849,
310.184642414137));
#12846=CARTESIAN_POINT('Ctrl Pts',(-32.5283098034614,-2.02924683297065,
310.18283936426));
#12847=CARTESIAN_POINT('Ctrl Pts',(-32.5398015859561,-2.03615576203388,
310.181940655409));
#12848=CARTESIAN_POINT('Ctrl Pts',(-32.5702890977271,-2.05413480949034,
310.179584081289));
#12849=CARTESIAN_POINT('Ctrl Pts',(-32.5893817081587,-2.06503919017128,
310.17813634446));
#12850=CARTESIAN_POINT('Ctrl Pts',(-32.6982681886916,-2.12523524382535,
310.17002116307));
#12851=CARTESIAN_POINT('Ctrl Pts',(-32.791039864022,-2.16894027257489,310.163642523094));
#12852=CARTESIAN_POINT('Ctrl Pts',(-33.010013260102,-2.25525587068017,310.149146265593));
#12853=CARTESIAN_POINT('Ctrl Pts',(-33.1375441976546,-2.29351680066534,
310.141092421946));
#12854=CARTESIAN_POINT('Ctrl Pts',(-33.3420126780833,-2.33655489296651,
310.128036637481));
#12855=CARTESIAN_POINT('Ctrl Pts',(-33.4171214203097,-2.34862788633159,
310.123214762106));
#12856=CARTESIAN_POINT('Ctrl Pts',(-33.5226563965961,-2.3604236123529,310.116324136595));
#12857=CARTESIAN_POINT('Ctrl Pts',(-33.5526976167911,-2.36320217159593,
310.114350012421));
#12858=CARTESIAN_POINT('Ctrl Pts',(-33.6050885953104,-2.36704154711581,
310.110880929024));
#12859=CARTESIAN_POINT('Ctrl Pts',(-33.6274159413871,-2.36836054930079,
310.109394249748));
#12860=CARTESIAN_POINT('Ctrl Pts',(-33.6739188965614,-2.37044823043038,
310.106279035273));
#12861=CARTESIAN_POINT('Ctrl Pts',(-33.6980941896539,-2.37116323858992,
310.104648989197));
#12862=CARTESIAN_POINT('Ctrl Pts',(-33.7622348184521,-2.37207880041941,
310.100294384748));
#12863=CARTESIAN_POINT('Ctrl Pts',(-33.8021999788263,-2.37163911379809,
310.097550256542));
#12864=CARTESIAN_POINT('Ctrl Pts',(-34.0346691661393,-2.36320361995575,
310.081399749584));
#12865=CARTESIAN_POINT('Ctrl Pts',(-34.2256086487502,-2.33278338072927,
310.067296242362));
#12866=CARTESIAN_POINT('Ctrl Pts',(-34.4981928041521,-2.2545106110892,310.046623919629));
#12867=CARTESIAN_POINT('Ctrl Pts',(-34.5841519206054,-2.22437800336578,
310.040036786114));
#12868=CARTESIAN_POINT('Ctrl Pts',(-34.6919713809225,-2.17946278782804,
310.031844271626));
#12869=CARTESIAN_POINT('Ctrl Pts',(-34.715607614713,-2.16916109030955,310.030052994054));
#12870=CARTESIAN_POINT('Ctrl Pts',(-34.7519982980303,-2.15258918511878,
310.027307527367));
#12871=CARTESIAN_POINT('Ctrl Pts',(-34.7648715433247,-2.14658666615213,
310.02633876429));
#12872=CARTESIAN_POINT('Ctrl Pts',(-34.7891068588569,-2.13502008099317,
310.024520679855));
#12873=CARTESIAN_POINT('Ctrl Pts',(-34.8004794344954,-2.12948024999071,
310.023670062994));
#12874=CARTESIAN_POINT('Ctrl Pts',(-34.8258863576674,-2.11685148829953,
310.021774435141));
#12875=CARTESIAN_POINT('Ctrl Pts',(-34.8398958554453,-2.1097133474959,310.020732376939));
#12876=CARTESIAN_POINT('Ctrl Pts',(-34.8898555805891,-2.08362878467335,
310.017024047034));
#12877=CARTESIAN_POINT('Ctrl Pts',(-34.9253905723551,-2.06389742002811,
310.014400970146));
#12878=CARTESIAN_POINT('Ctrl Pts',(-34.9931603596588,-2.023954634972,310.00939247732));
#12879=CARTESIAN_POINT('Ctrl Pts',(-35.0254498462756,-2.00386218565342,
310.007003390462));
#12880=CARTESIAN_POINT('Ctrl Pts',(-35.1895291822863,-1.89620398754174,
309.994775976132));
#12881=CARTESIAN_POINT('Ctrl Pts',(-35.3127987851945,-1.79638725481243,
309.985265583974));
#12882=CARTESIAN_POINT('Ctrl Pts',(-35.4837163132796,-1.6270875709388,309.970281224965));
#12883=CARTESIAN_POINT('Ctrl Pts',(-35.5391561431348,-1.56613657863932,
309.965075060634));
#12884=CARTESIAN_POINT('Ctrl Pts',(-35.6109034908421,-1.47849887648018,
309.957733631995));
#12885=CARTESIAN_POINT('Ctrl Pts',(-35.6300252628258,-1.45418702860978,
309.955711518031));
#12886=CARTESIAN_POINT('Ctrl Pts',(-35.6622151622646,-1.41157056585536,
309.952186948418));
#12887=CARTESIAN_POINT('Ctrl Pts',(-35.6755087130556,-1.39344082244651,
309.950693585776));
#12888=CARTESIAN_POINT('Ctrl Pts',(-35.7023994313485,-1.35565224532729,
309.947591621277));
#12889=CARTESIAN_POINT('Ctrl Pts',(-35.7159610958578,-1.33597141879378,
309.945981881709));
#12890=CARTESIAN_POINT('Ctrl Pts',(-35.7506051559474,-1.28403267474382,
309.941746880429));
#12891=CARTESIAN_POINT('Ctrl Pts',(-35.771202121143,-1.2514611374297,309.939103948812));
#12892=CARTESIAN_POINT('Ctrl Pts',(-35.8937173743332,-1.04684719610391,
309.922570431501));
#12893=CARTESIAN_POINT('Ctrl Pts',(-35.9743155376931,-0.863013479281199,
309.907914220209));
#12894=CARTESIAN_POINT('Ctrl Pts',(-36.0575260875028,-0.581047003459746,
309.886500232778));
#12895=CARTESIAN_POINT('Ctrl Pts',(-36.0787686025283,-0.489278039980603,
309.879703371807));
#12896=CARTESIAN_POINT('Ctrl Pts',(-36.0981141772791,-0.37518124770799,
309.871633084149));
#12897=CARTESIAN_POINT('Ctrl Pts',(-36.1014346233969,-0.353832082105871,
309.870139296852));
#12898=CARTESIAN_POINT('Ctrl Pts',(-36.1063310679241,-0.31924385277318,
309.867748600777));
#12899=CARTESIAN_POINT('Ctrl Pts',(-36.1080879124043,-0.306032168361609,
309.866842336293));
#12900=CARTESIAN_POINT('Ctrl Pts',(-36.1111846713285,-0.281140080896377,
309.865148723406));
#12901=CARTESIAN_POINT('Ctrl Pts',(-36.1125492768417,-0.269463260520901,
309.864359978435));
#12902=CARTESIAN_POINT('Ctrl Pts',(-36.1160241749421,-0.237680810853592,
309.86222751003));
#12903=CARTESIAN_POINT('Ctrl Pts',(-36.117964386681,-0.21755705313128,309.86089290033));
#12904=CARTESIAN_POINT('Ctrl Pts',(-36.1250835619893,-0.132321735545387,
309.85529666732));
#12905=CARTESIAN_POINT('Ctrl Pts',(-36.127829502897,-0.0670302973384229,
309.851149010829));
#12906=CARTESIAN_POINT('Ctrl Pts',(-36.1279901248444,0.15664866291237,309.837165036705));
#12907=CARTESIAN_POINT('Ctrl Pts',(-36.1122453066982,0.314617161043366,
309.82765056468));
#12908=CARTESIAN_POINT('Ctrl Pts',(-36.0637290767035,0.554671677968412,
309.812434591545));
#12909=CARTESIAN_POINT('Ctrl Pts',(-36.041956299146,0.638490476428677,309.806978345435));
#12910=CARTESIAN_POINT('Ctrl Pts',(-36.0058908939347,0.751526639243565,
309.799299896309));
#12911=CARTESIAN_POINT('Ctrl Pts',(-35.9955073882524,0.781924025417422,
309.797202709811));
#12912=CARTESIAN_POINT('Ctrl Pts',(-35.9768223499762,0.833195326432809,
309.793604928395));
#12913=CARTESIAN_POINT('Ctrl Pts',(-35.9688355628786,0.854179750292814,
309.792114921734));
#12914=CARTESIAN_POINT('Ctrl Pts',(-35.9518895487267,0.896870280810288,
309.789046041881));
#12915=CARTESIAN_POINT('Ctrl Pts',(-35.9429034979679,0.918562980672566,
309.787466397287));
#12916=CARTESIAN_POINT('Ctrl Pts',(-35.9191653445074,0.973544502085842,
309.78340905261));
#12917=CARTESIAN_POINT('Ctrl Pts',(-35.9039665027997,1.00663250020668,309.780916374907));
#12918=CARTESIAN_POINT('Ctrl Pts',(-35.8689862834002,1.07838253660604,309.77539523487));
#12919=CARTESIAN_POINT('Ctrl Pts',(-35.8488927916008,1.11687697673336,309.772357032586));
#12920=CARTESIAN_POINT('Ctrl Pts',(-35.7820062703195,1.23686697344908,309.762643709851));
#12921=CARTESIAN_POINT('Ctrl Pts',(-35.7314247626472,1.3161392637049,309.755857333316));
#12922=CARTESIAN_POINT('Ctrl Pts',(-35.584849297343,1.51829988738251,309.737663284056));
#12923=CARTESIAN_POINT('Ctrl Pts',(-35.4812135343735,1.6350971198002,309.726177842687));
#12924=CARTESIAN_POINT('Ctrl Pts',(-35.3490517307395,1.75737818226608,309.713573402676));
#12925=CARTESIAN_POINT('Ctrl Pts',(-35.3309828979073,1.7735885340657,309.711889712769));
#12926=CARTESIAN_POINT('Ctrl Pts',(-35.302186875315,1.79863558047589,309.709272100488));
#12927=CARTESIAN_POINT('Ctrl Pts',(-35.2916259955825,1.80765979877798,309.708325589834));
#12928=CARTESIAN_POINT('Ctrl Pts',(-35.2710706828736,1.82491407084933,309.706510234453));
#12929=CARTESIAN_POINT('Ctrl Pts',(-35.2610872020172,1.83315589274702,309.705640638796));
#12930=CARTESIAN_POINT('Ctrl Pts',(-35.2357418108779,1.85373306285923,309.703461926363));
#12931=CARTESIAN_POINT('Ctrl Pts',(-35.2202923185473,1.86595987085937,309.702160255518));
#12932=CARTESIAN_POINT('Ctrl Pts',(-35.1535232965387,1.91746125030801,309.696637764405));
#12933=CARTESIAN_POINT('Ctrl Pts',(-35.1007583533388,1.95482534751463,309.692529715554));
#12934=CARTESIAN_POINT('Ctrl Pts',(-34.9209647787354,2.07141176346231,309.679121170559));
#12935=CARTESIAN_POINT('Ctrl Pts',(-34.7879732710474,2.14076875919909,309.670111006596));
#12936=CARTESIAN_POINT('Ctrl Pts',(-34.6294057650476,2.20523122917619,309.659512528632));
#12937=CARTESIAN_POINT('Ctrl Pts',(-34.6093750269977,2.21305859674719,309.658176665385));
#12938=CARTESIAN_POINT('Ctrl Pts',(-34.5164118667015,2.24793586736593,309.651982829893));
#12939=CARTESIAN_POINT('Ctrl Pts',(-34.4422891007593,2.27165765831294,309.647058934433));
#12940=CARTESIAN_POINT('Ctrl Pts',(-34.3370435804155,2.29971828706415,309.640000871605));
#12941=CARTESIAN_POINT('Ctrl Pts',(-34.3067932792655,2.3071486236396,309.637964966859));
#12942=CARTESIAN_POINT('Ctrl Pts',(-34.2544394194209,2.31891995768009,309.634424325861));
#12943=CARTESIAN_POINT('Ctrl Pts',(-34.2324037432807,2.32354587658817,309.632928918703));
#12944=CARTESIAN_POINT('Ctrl Pts',(-34.1869208595193,2.33241986476121,309.629830098033));
#12945=CARTESIAN_POINT('Ctrl Pts',(-34.1634688906183,2.33662968519359,309.628225647786));
#12946=CARTESIAN_POINT('Ctrl Pts',(-34.1022997063071,2.34666121141518,309.624021795088));
#12947=CARTESIAN_POINT('Ctrl Pts',(-34.0644996728687,2.35192695081531,309.62140520576));
#12948=CARTESIAN_POINT('Ctrl Pts',(-33.8919688502865,2.37173078929483,309.609370475106));
#12949=CARTESIAN_POINT('Ctrl Pts',(-33.756290696015,2.37561561810063,309.599632185729));
#12950=CARTESIAN_POINT('Ctrl Pts',(-33.4675075478428,2.35914108231101,309.578551909545));
#12951=CARTESIAN_POINT('Ctrl Pts',(-33.3151791031411,2.33546977943752,309.567217484439));
#12952=CARTESIAN_POINT('Ctrl Pts',(-33.1424761454034,2.29112002416459,309.554731548541));
#12953=CARTESIAN_POINT('Ctrl Pts',(-33.1188396788813,2.28465825093942,309.553031529024));
#12954=CARTESIAN_POINT('Ctrl Pts',(-33.0819199664729,2.27394748943518,309.550394472026));
#12955=CARTESIAN_POINT('Ctrl Pts',(-33.0685675297594,2.26994588214746,309.549444552077));
#12956=CARTESIAN_POINT('Ctrl Pts',(-33.0429083355688,2.26200885794384,309.547627481613));
#12957=CARTESIAN_POINT('Ctrl Pts',(-33.0305972661729,2.2580902439807,309.546759515801));
#12958=CARTESIAN_POINT('Ctrl Pts',(-32.9997299133956,2.24798666186072,309.54459165892));
#12959=CARTESIAN_POINT('Ctrl Pts',(-32.9812164482368,2.24167220678584,309.54329905416));
#12960=CARTESIAN_POINT('Ctrl Pts',(-32.903340755563,2.21403073670725,309.537885645701));
#12961=CARTESIAN_POINT('Ctrl Pts',(-32.8447587004936,2.19056745362947,309.533872113895));
#12962=CARTESIAN_POINT('Ctrl Pts',(-32.7475764827858,2.14706921873693,309.527203448312));
#12963=CARTESIAN_POINT('Ctrl Pts',(-32.7084862560888,2.12826834459275,309.524518071325));
#12964=CARTESIAN_POINT('Ctrl Pts',(-32.6699489539077,2.1084153432895,309.521847592916));
#12965=CARTESIAN_POINT('',(-36.1278762480309,-0.000944544423845245,309.649405795056));
#12966=CARTESIAN_POINT('Ctrl Pts',(-32.6699490796625,2.10841540807375,309.323530658174));
#12967=CARTESIAN_POINT('Ctrl Pts',(-32.6837670278073,2.11553390591377,309.324574657703));
#12968=CARTESIAN_POINT('Ctrl Pts',(-32.6976545041501,2.12251633343421,309.325623441197));
#12969=CARTESIAN_POINT('Ctrl Pts',(-32.7450521640656,2.14576634592794,309.329201953145));
#12970=CARTESIAN_POINT('Ctrl Pts',(-32.7788748771904,2.16138001081334,309.331754045084));
#12971=CARTESIAN_POINT('Ctrl Pts',(-32.8541195406299,2.19398816596706,309.33743146526));
#12972=CARTESIAN_POINT('Ctrl Pts',(-32.8956826396133,2.21061905175698,309.340567493712));
#12973=CARTESIAN_POINT('Ctrl Pts',(-33.0308283563419,2.26030693599979,309.350762875372));
#12974=CARTESIAN_POINT('Ctrl Pts',(-33.1260166795685,2.28866845150412,309.357946347631));
#12975=CARTESIAN_POINT('Ctrl Pts',(-33.3644469287239,2.34370424693655,309.375795128266));
#12976=CARTESIAN_POINT('Ctrl Pts',(-33.5089202630452,2.36331499526615,309.38649634971));
#12977=CARTESIAN_POINT('Ctrl Pts',(-33.679639658142,2.37065215195957,309.398475664489));
#12978=CARTESIAN_POINT('Ctrl Pts',(-33.7050082096984,2.37133484339931,309.400237987235));
#12979=CARTESIAN_POINT('Ctrl Pts',(-33.7445023091299,2.37176353723193,309.402949064332));
#12980=CARTESIAN_POINT('Ctrl Pts',(-33.7586220923958,2.37179071821195,309.40391184773));
#12981=CARTESIAN_POINT('Ctrl Pts',(-33.7855711077937,2.37160192899248,309.405736002992));
#12982=CARTESIAN_POINT('Ctrl Pts',(-33.7983995662419,2.37140795800151,309.406598428723));
#12983=CARTESIAN_POINT('Ctrl Pts',(-33.8302816621777,2.37066709246916,309.40872826764));
#12984=CARTESIAN_POINT('Ctrl Pts',(-33.849331968908,2.36999457172687,309.409988950329));
#12985=CARTESIAN_POINT('Ctrl Pts',(-33.9263358677854,2.36634618465872,309.415043980755));
#12986=CARTESIAN_POINT('Ctrl Pts',(-33.9841837939127,2.36147339752557,309.418748075766));
#12987=CARTESIAN_POINT('Ctrl Pts',(-34.1592156250369,2.34023655905682,309.429827470924));
#12988=CARTESIAN_POINT('Ctrl Pts',(-34.2754079031037,2.31722637098704,309.437012990825));
#12989=CARTESIAN_POINT('Ctrl Pts',(-34.5147457740534,2.25091366793179,309.452257173774));
#12990=CARTESIAN_POINT('Ctrl Pts',(-34.6370043581484,2.20593839645373,309.46031087037));
#12991=CARTESIAN_POINT('Ctrl Pts',(-34.786648644744,2.13645605753466,309.470950817336));
#12992=CARTESIAN_POINT('Ctrl Pts',(-34.818014148158,2.12104097693873,309.473225980454));
#12993=CARTESIAN_POINT('Ctrl Pts',(-34.8696117392651,2.09425114209687,309.477051216784));
#12994=CARTESIAN_POINT('Ctrl Pts',(-34.8900385637574,2.08326201249233,309.478587651));
#12995=CARTESIAN_POINT('Ctrl Pts',(-34.930326706358,2.06081990278973,309.48166402222));
#12996=CARTESIAN_POINT('Ctrl Pts',(-34.9501896520774,2.04937501252228,309.483203544001));
#12997=CARTESIAN_POINT('Ctrl Pts',(-34.9986690005221,2.02049750079732,309.487019258701));
#12998=CARTESIAN_POINT('Ctrl Pts',(-35.0270870577989,2.0027433950187,309.489306995416));
#12999=CARTESIAN_POINT('Ctrl Pts',(-35.1481737362104,1.9234796334618,309.4992832111));
#13000=CARTESIAN_POINT('Ctrl Pts',(-35.236816040945,1.85610390644244,309.507186323455));
#13001=CARTESIAN_POINT('Ctrl Pts',(-35.3910244388719,1.72079562743263,309.522031054723));
#13002=CARTESIAN_POINT('Ctrl Pts',(-35.457906786202,1.65468179327469,309.528916817575));
#13003=CARTESIAN_POINT('Ctrl Pts',(-35.5864278181724,1.51158079860509,309.542937993197));
#13004=CARTESIAN_POINT('Ctrl Pts',(-35.6475558899725,1.43435641010294,309.550056579666));
#13005=CARTESIAN_POINT('Ctrl Pts',(-35.7162397633653,1.3355290221792,309.558453820506));
#13006=CARTESIAN_POINT('Ctrl Pts',(-35.7285144458637,1.31733354366597,309.55997197576));
#13007=CARTESIAN_POINT('Ctrl Pts',(-35.7478739155931,1.28775849014213,309.562391805709));
#13008=CARTESIAN_POINT('Ctrl Pts',(-35.7551175980459,1.27648514147036,309.563303231245));
#13009=CARTESIAN_POINT('Ctrl Pts',(-35.7693628508485,1.25389656633207,309.565106792945));
#13010=CARTESIAN_POINT('Ctrl Pts',(-35.7763655046659,1.24258263102299,309.565998972036));
#13011=CARTESIAN_POINT('Ctrl Pts',(-35.7944343383787,1.21283290666031,309.568317518116));
#13012=CARTESIAN_POINT('Ctrl Pts',(-35.8053459783039,1.19430403396777,309.569734341045));
#13013=CARTESIAN_POINT('Ctrl Pts',(-35.8615069496667,1.0959015860009,309.577130488354));
#13014=CARTESIAN_POINT('Ctrl Pts',(-35.9023475588104,1.0135907143416,309.582878455362));
#13015=CARTESIAN_POINT('Ctrl Pts',(-35.9725480215865,0.848711841000923,
309.593950944079));
#13016=CARTESIAN_POINT('Ctrl Pts',(-36.0023104729367,0.766481700466652,
309.599274457109));
#13017=CARTESIAN_POINT('Ctrl Pts',(-36.0479015141048,0.614821737788254,
309.609006589604));
#13018=CARTESIAN_POINT('Ctrl Pts',(-36.0652728854282,0.545967628761038,
309.613393822181));
#13019=CARTESIAN_POINT('Ctrl Pts',(-36.0925180552505,0.413104409625198,
309.621918089787));
#13020=CARTESIAN_POINT('Ctrl Pts',(-36.1029097526244,0.349267828244329,
309.626038783868));
#13021=CARTESIAN_POINT('Ctrl Pts',(-36.1141506117227,0.256429903997621,
309.632115709324));
#13022=CARTESIAN_POINT('Ctrl Pts',(-36.1170971204671,0.227709507052592,
309.634007040841));
#13023=CARTESIAN_POINT('Ctrl Pts',(-36.1213347166058,0.177368079683672,
309.637345736844));
#13024=CARTESIAN_POINT('Ctrl Pts',(-36.122855290686,0.155769455874528,309.638785727079));
#13025=CARTESIAN_POINT('Ctrl Pts',(-36.1253583088053,0.111588552168876,
309.641748104397));
#13026=CARTESIAN_POINT('Ctrl Pts',(-36.1263140563778,0.0890070546941616,
309.643271178472));
#13027=CARTESIAN_POINT('Ctrl Pts',(-36.1275758177347,0.0439665759513204,
309.646328070369));
#13028=CARTESIAN_POINT('Ctrl Pts',(-36.1278857981901,0.0215101600079903,
309.647861594863));
#13029=CARTESIAN_POINT('Ctrl Pts',(-36.1278768363983,-0.000946495695927301,
309.649404906755));
#13030=CARTESIAN_POINT('Ctrl Pts',(-36.1278768371482,-0.000944614581569902,
309.649404777478));
#13031=CARTESIAN_POINT('Ctrl Pts',(-36.1278663893725,-0.0271770173666605,
309.651207573291));
#13032=CARTESIAN_POINT('Ctrl Pts',(-36.127420733878,-0.0534067147285239,
309.653023524514));
#13033=CARTESIAN_POINT('Ctrl Pts',(-36.1194844509716,-0.289673589458124,
309.669503194538));
#13034=CARTESIAN_POINT('Ctrl Pts',(-36.0845391621194,-0.497831258028484,
309.685015777814));
#13035=CARTESIAN_POINT('Ctrl Pts',(-36.0075251207054,-0.747691639858987,
309.703970158497));
#13036=CARTESIAN_POINT('Ctrl Pts',(-35.9908047306328,-0.796274034546403,
309.707665456643));
#13037=CARTESIAN_POINT('Ctrl Pts',(-35.9600788646211,-0.87693536270526,
309.713779306713));
#13038=CARTESIAN_POINT('Ctrl Pts',(-35.9469176782966,-0.909316207975562,
309.716227594138));
#13039=CARTESIAN_POINT('Ctrl Pts',(-35.9267201011362,-0.956021792803638,
309.719738387782));
#13040=CARTESIAN_POINT('Ctrl Pts',(-35.9202479323392,-0.970583692846614,
309.720830012436));
#13041=CARTESIAN_POINT('Ctrl Pts',(-35.9089485757408,-0.995331320502093,
309.722678749617));
#13042=CARTESIAN_POINT('Ctrl Pts',(-35.904194918026,-1.00554930731328,309.72344009382));
#13043=CARTESIAN_POINT('Ctrl Pts',(-35.8927618201674,-1.02967362877591,
309.725232923355));
#13044=CARTESIAN_POINT('Ctrl Pts',(-35.8860192958682,-1.04354922102529,
309.726260561577));
#13045=CARTESIAN_POINT('Ctrl Pts',(-35.8648396596177,-1.08607470020187,
309.729402105718));
#13046=CARTESIAN_POINT('Ctrl Pts',(-35.8499556748801,-1.11449946476577,
309.731490788564));
#13047=CARTESIAN_POINT('Ctrl Pts',(-35.7375741958693,-1.31891692569195,
309.746493594965));
#13048=CARTESIAN_POINT('Ctrl Pts',(-35.618601789144,-1.48218826075821,309.758438393318));
#13049=CARTESIAN_POINT('Ctrl Pts',(-35.4189706264659,-1.69356455869197,
309.77648994116));
#13050=CARTESIAN_POINT('Ctrl Pts',(-35.3538841758165,-1.75510093005289,
309.782130338333));
#13051=CARTESIAN_POINT('Ctrl Pts',(-35.261251713375,-1.83324919970288,309.789977731786));
#13052=CARTESIAN_POINT('Ctrl Pts',(-35.2366159366122,-1.85320138724587,
309.792048450123));
#13053=CARTESIAN_POINT('Ctrl Pts',(-35.1937405110199,-1.88652498316338,
309.795629794204));
#13054=CARTESIAN_POINT('Ctrl Pts',(-35.1756955497267,-1.90014057129233,
309.797130488479));
#13055=CARTESIAN_POINT('Ctrl Pts',(-35.1383784904002,-1.92746939987681,
309.800222268681));
#13056=CARTESIAN_POINT('Ctrl Pts',(-35.119090414151,-1.94115638997271,309.801814146026));
#13057=CARTESIAN_POINT('Ctrl Pts',(-35.0688787739199,-1.97566969418307,
309.805944240345));
#13058=CARTESIAN_POINT('Ctrl Pts',(-35.0376640581931,-1.99605872971316,
309.808498521476));
#13059=CARTESIAN_POINT('Ctrl Pts',(-34.8308610769926,-2.12428895000816,
309.825345307427));
#13060=CARTESIAN_POINT('Ctrl Pts',(-34.6423601482496,-2.20957364562771,
309.840463857755));
#13061=CARTESIAN_POINT('Ctrl Pts',(-34.3584009067633,-2.2958018602168,309.862065697617));
#13062=CARTESIAN_POINT('Ctrl Pts',(-34.2700802934869,-2.31717401524013,
309.86861459548));
#13063=CARTESIAN_POINT('Ctrl Pts',(-34.1596361441523,-2.33727164295446,
309.876441278761));
#13064=CARTESIAN_POINT('Ctrl Pts',(-34.1384765476125,-2.34082619314409,
309.877924424734));
#13065=CARTESIAN_POINT('Ctrl Pts',(-34.1041305850791,-2.3461177178856,309.880302347643));
#13066=CARTESIAN_POINT('Ctrl Pts',(-34.0909732178138,-2.34803170234124,
309.8812063107));
#13067=CARTESIAN_POINT('Ctrl Pts',(-34.0645141153359,-2.35165373469032,
309.883009217015));
#13068=CARTESIAN_POINT('Ctrl Pts',(-34.051212625637,-2.35335981013539,309.883908031345));
#13069=CARTESIAN_POINT('Ctrl Pts',(-34.0160567011594,-2.35756621374573,
309.886265424643));
#13070=CARTESIAN_POINT('Ctrl Pts',(-33.9941801606791,-2.35987556439513,
309.887713861324));
#13071=CARTESIAN_POINT('Ctrl Pts',(-33.8679243399572,-2.37142982273592,
309.89598317123));
#13072=CARTESIAN_POINT('Ctrl Pts',(-33.7630436674355,-2.374054647722,309.902501216431));
#13073=CARTESIAN_POINT('Ctrl Pts',(-33.527239143176,-2.36432241042568,309.917028335508));
#13074=CARTESIAN_POINT('Ctrl Pts',(-33.3968350491521,-2.34804567742497,
309.924982527676));
#13075=CARTESIAN_POINT('Ctrl Pts',(-33.1945207636331,-2.3055374268082,309.937903165899));
#13076=CARTESIAN_POINT('Ctrl Pts',(-33.1213851253045,-2.2864832071445,309.942694815755));
#13077=CARTESIAN_POINT('Ctrl Pts',(-33.0205524130896,-2.25500205691276,
309.949549776262));
#13078=CARTESIAN_POINT('Ctrl Pts',(-32.9919913588175,-2.2454845434132,309.951519841096));
#13079=CARTESIAN_POINT('Ctrl Pts',(-32.9425498621689,-2.227956467529,309.954984178094));
#13080=CARTESIAN_POINT('Ctrl Pts',(-32.9215868187212,-2.22018927273224,
309.956470237377));
#13081=CARTESIAN_POINT('Ctrl Pts',(-32.8781578490868,-2.20339607223984,
309.959586476187));
#13082=CARTESIAN_POINT('Ctrl Pts',(-32.85571416559,-2.19432010697264,309.961218198427));
#13083=CARTESIAN_POINT('Ctrl Pts',(-32.7964851949182,-2.16930693556733,
309.965583055382));
#13084=CARTESIAN_POINT('Ctrl Pts',(-32.7599597643281,-2.15277854667102,
309.968335928514));
#13085=CARTESIAN_POINT('Ctrl Pts',(-32.5838841110795,-2.06766074668186,
309.981915675507));
#13086=CARTESIAN_POINT('Ctrl Pts',(-32.4509112286364,-1.98639660849529,
309.993171890676));
#13087=CARTESIAN_POINT('Ctrl Pts',(-32.253541058487,-1.83735563336454,310.011235144592));
#13088=CARTESIAN_POINT('Ctrl Pts',(-32.1834932737139,-1.77776961265017,
310.017955747456));
#13089=CARTESIAN_POINT('Ctrl Pts',(-32.0804507354419,-1.67924830097529,
310.028173344617));
#13090=CARTESIAN_POINT('Ctrl Pts',(-32.0449531490419,-1.64306137473039,
310.031760900384));
#13091=CARTESIAN_POINT('Ctrl Pts',(-31.9982978420506,-1.59234635901782,
310.036538875745));
#13092=CARTESIAN_POINT('Ctrl Pts',(-31.9861106257484,-1.57878825748567,
310.037793120951));
#13093=CARTESIAN_POINT('Ctrl Pts',(-31.9657028575972,-1.55555152222233,
310.039901948594));
#13094=CARTESIAN_POINT('Ctrl Pts',(-31.9574016961712,-1.54594516736175,
310.040762180356));
#13095=CARTESIAN_POINT('Ctrl Pts',(-31.9397977724989,-1.52523958824999,
310.042591147213));
#13096=CARTESIAN_POINT('Ctrl Pts',(-31.9305189420888,-1.51412116755396,
310.043558238648));
#13097=CARTESIAN_POINT('Ctrl Pts',(-31.9046184925332,-1.48250151298038,
310.046268772998));
#13098=CARTESIAN_POINT('Ctrl Pts',(-31.8882358470808,-1.461806167278,310.047996394486));
#13099=CARTESIAN_POINT('Ctrl Pts',(-31.8134171943242,-1.36397939543674,
310.055971946254));
#13100=CARTESIAN_POINT('Ctrl Pts',(-31.7593855440788,-1.2835842972397,310.06198562576));
#13101=CARTESIAN_POINT('Ctrl Pts',(-31.6441839097512,-1.08721012277575,
310.075998394509));
#13102=CARTESIAN_POINT('Ctrl Pts',(-31.5874157525307,-0.969030480296554,
310.083934788113));
#13103=CARTESIAN_POINT('Ctrl Pts',(-31.5137490814012,-0.776293830706618,
310.096831249294));
#13104=CARTESIAN_POINT('Ctrl Pts',(-31.4901919021824,-0.704575967787306,
310.101617453138));
#13105=CARTESIAN_POINT('Ctrl Pts',(-31.4620768529805,-0.602857700253395,
310.108466000096));
#13106=CARTESIAN_POINT('Ctrl Pts',(-31.4546129942304,-0.573704304930778,
310.110435345184));
#13107=CARTESIAN_POINT('Ctrl Pts',(-31.4425749595652,-0.522661064059756,
310.113898856752));
#13108=CARTESIAN_POINT('Ctrl Pts',(-31.4377518384465,-0.500833488618011,
310.115384822435));
#13109=CARTESIAN_POINT('Ctrl Pts',(-31.4283485340707,-0.455227029343866,
310.118501295058));
#13110=CARTESIAN_POINT('Ctrl Pts',(-31.4238225814206,-0.431439749840212,
310.120133350641));
#13111=CARTESIAN_POINT('Ctrl Pts',(-31.4127687215022,-0.368074405734188,
310.124500173513));
#13112=CARTESIAN_POINT('Ctrl Pts',(-31.406879561581,-0.328394459872724,
310.127254711164));
#13113=CARTESIAN_POINT('Ctrl Pts',(-31.3831548633909,-0.134861487227556,
310.140793920795));
#13114=CARTESIAN_POINT('Ctrl Pts',(-31.3794155838814,0.0203158112070516,
310.152004045879));
#13115=CARTESIAN_POINT('Ctrl Pts',(-31.3976201757656,0.266758500495503,
310.170051719646));
#13116=CARTESIAN_POINT('Ctrl Pts',(-31.4097848335549,0.35832161174487,310.176802578874));
#13117=CARTESIAN_POINT('Ctrl Pts',(-31.4368709361756,0.498828620726649,
310.187059023653));
#13118=CARTESIAN_POINT('Ctrl Pts',(-31.4480879953059,0.548393537905482,
310.190655855371));
#13119=CARTESIAN_POINT('Ctrl Pts',(-31.4654861596984,0.615219763046917,
310.195443879524));
#13120=CARTESIAN_POINT('Ctrl Pts',(-31.4702866823658,0.632822969589049,
310.196699227583));
#13121=CARTESIAN_POINT('Ctrl Pts',(-31.4787719784252,0.662580777982345,
310.198809314407));
#13122=CARTESIAN_POINT('Ctrl Pts',(-31.4823520233285,0.67476408387007,310.199669719198));
#13123=CARTESIAN_POINT('Ctrl Pts',(-31.4902218096407,0.700771782705733,
310.201498367107));
#13124=CARTESIAN_POINT('Ctrl Pts',(-31.4945404827555,0.714586506803554,
310.202464976092));
#13125=CARTESIAN_POINT('Ctrl Pts',(-31.5070794391263,0.753443870667212,
310.205172723694));
#13126=CARTESIAN_POINT('Ctrl Pts',(-31.5155913363286,0.778391083264248,
310.206898092016));
#13127=CARTESIAN_POINT('Ctrl Pts',(-31.5810619047284,0.960296086317004,
310.219418400276));
#13128=CARTESIAN_POINT('Ctrl Pts',(-31.6540451703501,1.11101001867177,310.229484184463));
#13129=CARTESIAN_POINT('Ctrl Pts',(-31.8040129845266,1.35207740946097,310.246923069845));
#13130=CARTESIAN_POINT('Ctrl Pts',(-31.873007030978,1.44662277081856,310.254168720521));
#13131=CARTESIAN_POINT('Ctrl Pts',(-31.9739480148236,1.56542595776726,310.26417726903));
#13132=CARTESIAN_POINT('Ctrl Pts',(-31.9999404314216,1.59453090930713,310.266708295609));
#13133=CARTESIAN_POINT('Ctrl Pts',(-32.0430578587427,1.64047794353478,310.270844056999));
#13134=CARTESIAN_POINT('Ctrl Pts',(-32.0597420477038,1.65772488347278,310.272430019407));
#13135=CARTESIAN_POINT('Ctrl Pts',(-32.0925273976463,1.69060277795411,310.275521214851));
#13136=CARTESIAN_POINT('Ctrl Pts',(-32.108594411927,1.70626425323569,310.277024843648));
#13137=CARTESIAN_POINT('Ctrl Pts',(-32.1471329331801,1.74277816592017,310.280606732503));
#13138=CARTESIAN_POINT('Ctrl Pts',(-32.1697908189261,1.76342706415366,310.282693405203));
#13139=CARTESIAN_POINT('Ctrl Pts',(-32.2486176057592,1.83251580399968,310.289892003041));
#13140=CARTESIAN_POINT('Ctrl Pts',(-32.3066502320305,1.87875326611189,310.295090775305));
#13141=CARTESIAN_POINT('Ctrl Pts',(-32.3897864074735,1.93884487102298,310.302401196712));
#13142=CARTESIAN_POINT('Ctrl Pts',(-32.4131214640902,1.95508109611666,310.304438789964));
#13143=CARTESIAN_POINT('Ctrl Pts',(-32.5118214152301,2.02115428894747,310.31299357935));
#13144=CARTESIAN_POINT('Ctrl Pts',(-32.5896863653336,2.06706702007088,310.319594316565));
#13145=CARTESIAN_POINT('Ctrl Pts',(-32.6699491957805,2.10841546789345,310.326187962698));
#13146=CARTESIAN_POINT('Origin',(-33.7561270252576,0.,302.151410108095));
#13147=CARTESIAN_POINT('',(-32.6714234043919,2.10551637491534,311.522951534327));
#13148=CARTESIAN_POINT('',(-32.6699490813724,2.10841540895464,311.327581625012));
#13149=CARTESIAN_POINT('',(-32.6699490794746,2.10841540797695,302.151410108095));
#13150=CARTESIAN_POINT('',(-36.1295666873539,0.00193988692732453,310.848590956866));
#13151=CARTESIAN_POINT('Ctrl Pts',(-36.1295666873539,0.00193988692732453,
310.848590956866));
#13152=CARTESIAN_POINT('Ctrl Pts',(-36.123741267486,-0.652989171154178,
310.892622454172));
#13153=CARTESIAN_POINT('Ctrl Pts',(-35.5020848627001,-2.10550375003854,
310.989624382201));
#13154=CARTESIAN_POINT('Ctrl Pts',(-33.0415486194394,-2.71176251122329,
311.139596740952));
#13155=CARTESIAN_POINT('Ctrl Pts',(-31.0894948106476,-0.867957931798494,
311.298508033121));
#13156=CARTESIAN_POINT('Ctrl Pts',(-31.485743561134,1.2545895519984,311.426292964246));
#13157=CARTESIAN_POINT('Ctrl Pts',(-32.3803640906792,1.95726749312548,311.501107464648));
#13158=CARTESIAN_POINT('Ctrl Pts',(-32.671423404392,2.10551637491536,311.522951534327));
#13159=CARTESIAN_POINT('Ctrl Pts',(-36.1278762772803,0.00188362146629249,
310.847619667516));
#13160=CARTESIAN_POINT('Ctrl Pts',(-36.1277997378554,0.0982577215860634,
310.840595642696));
#13161=CARTESIAN_POINT('Ctrl Pts',(-36.1218491037786,0.194549688000836,
310.833625037494));
#13162=CARTESIAN_POINT('Ctrl Pts',(-36.1080209960884,0.306706121591654,
310.825735930453));
#13163=CARTESIAN_POINT('Ctrl Pts',(-36.1058155576088,0.323168273179709,
310.824583945188));
#13164=CARTESIAN_POINT('Ctrl Pts',(-36.1016682989013,0.351833521843165,
310.822589966578));
#13165=CARTESIAN_POINT('Ctrl Pts',(-36.0998037388827,0.364046936929179,
310.821744189674));
#13166=CARTESIAN_POINT('Ctrl Pts',(-36.0960462957189,0.387432907720725,
310.820132716905));
#13167=CARTESIAN_POINT('Ctrl Pts',(-36.094168651592,0.398607355240138,310.819366282987));
#13168=CARTESIAN_POINT('Ctrl Pts',(-36.0896392315116,0.424429498608024,
310.817603671748));
#13169=CARTESIAN_POINT('Ctrl Pts',(-36.0869295557214,0.439066292826559,
310.816610727732));
#13170=CARTESIAN_POINT('Ctrl Pts',(-36.078497069862,0.482335942655559,310.813691011211));
#13171=CARTESIAN_POINT('Ctrl Pts',(-36.0723829181109,0.510890802250861,
310.811784569628));
#13172=CARTESIAN_POINT('Ctrl Pts',(-36.0345657394104,0.672839206118621,
310.801050717806));
#13173=CARTESIAN_POINT('Ctrl Pts',(-35.9918668587651,0.803412498934501,
310.792691078824));
#13174=CARTESIAN_POINT('Ctrl Pts',(-35.8971067513509,1.02584260222284,310.777875130296));
#13175=CARTESIAN_POINT('Ctrl Pts',(-35.8497712513038,1.11928509156068,310.771455128697));
#13176=CARTESIAN_POINT('Ctrl Pts',(-35.7943400030282,1.21280774330486,310.764606838929));
#13177=CARTESIAN_POINT('Ctrl Pts',(-35.792247143385,1.21631806254776,310.764349157966));
#13178=CARTESIAN_POINT('Ctrl Pts',(-35.7827524367733,1.23215020131538,310.763184059302));
#13179=CARTESIAN_POINT('Ctrl Pts',(-35.7752478381601,1.24440982341308,310.76227387106));
#13180=CARTESIAN_POINT('Ctrl Pts',(-35.7506094756113,1.28384972943842,310.75931843913));
#13181=CARTESIAN_POINT('Ctrl Pts',(-35.7330352625072,1.31074942298467,310.757260247393));
#13182=CARTESIAN_POINT('Ctrl Pts',(-35.6963836132923,1.36443515809161,310.75305762165));
#13183=CARTESIAN_POINT('Ctrl Pts',(-35.6772848134762,1.39119786771531,310.750912764556));
#13184=CARTESIAN_POINT('Ctrl Pts',(-35.6440031310601,1.43584198213507,310.747243621427));
#13185=CARTESIAN_POINT('Ctrl Pts',(-35.6301068964989,1.45393183092294,310.74573057365));
#13186=CARTESIAN_POINT('Ctrl Pts',(-35.6014690727268,1.49011928878912,310.74264831544));
#13187=CARTESIAN_POINT('Ctrl Pts',(-35.5867169562676,1.50820529229695,310.741078788821));
#13188=CARTESIAN_POINT('Ctrl Pts',(-35.5487380710858,1.55338897513909,310.73708163383));
#13189=CARTESIAN_POINT('Ctrl Pts',(-35.5251628388251,1.58018471022434,310.734639906718));
#13190=CARTESIAN_POINT('Ctrl Pts',(-35.369041358055,1.74975939878078,310.71870987128));
#13191=CARTESIAN_POINT('Ctrl Pts',(-35.2199549257829,1.87625430744034,310.70448638847));
#13192=CARTESIAN_POINT('Ctrl Pts',(-34.9766504722834,2.03587437760495,310.683257777607));
#13193=CARTESIAN_POINT('Ctrl Pts',(-34.8930273885534,2.08372811627144,310.676276576912));
#13194=CARTESIAN_POINT('Ctrl Pts',(-34.7830563528748,2.1380624209283,310.667666419169));
#13195=CARTESIAN_POINT('Ctrl Pts',(-34.7591973574047,2.14935916338813,310.665831277558));
#13196=CARTESIAN_POINT('Ctrl Pts',(-34.7221026816098,2.16617044613488,310.663033868942));
#13197=CARTESIAN_POINT('Ctrl Pts',(-34.7089980623794,2.17196689289468,310.662056186275));
#13198=CARTESIAN_POINT('Ctrl Pts',(-34.6841369345618,2.18269516261417,310.660222393903));
#13199=CARTESIAN_POINT('Ctrl Pts',(-34.6723925373103,2.18765127092185,310.65936499887));
#13200=CARTESIAN_POINT('Ctrl Pts',(-34.6461917601799,2.19845992163519,310.657470947976));
#13201=CARTESIAN_POINT('Ctrl Pts',(-34.6317167273268,2.20426494899861,310.656437057341));
#13202=CARTESIAN_POINT('Ctrl Pts',(-34.5802524042987,2.22431708960753,310.652801694868));
#13203=CARTESIAN_POINT('Ctrl Pts',(-34.5429623386241,2.23778009846736,310.650241165652));
#13204=CARTESIAN_POINT('Ctrl Pts',(-34.3716287900983,2.29482442428157,310.63873319389));
#13205=CARTESIAN_POINT('Ctrl Pts',(-34.2341935962218,2.32734205370379,310.630194931516));
#13206=CARTESIAN_POINT('Ctrl Pts',(-34.0081380273211,2.35994337252435,310.616175615873));
#13207=CARTESIAN_POINT('Ctrl Pts',(-33.9209827474776,2.36762821606296,310.610779000097));
#13208=CARTESIAN_POINT('Ctrl Pts',(-33.7738841194592,2.3724361644907,310.601492310927));
#13209=CARTESIAN_POINT('Ctrl Pts',(-33.7141133020573,2.37213039410012,310.59767020961));
#13210=CARTESIAN_POINT('Ctrl Pts',(-33.6266274857506,2.36837536131658,310.591967537359));
#13211=CARTESIAN_POINT('Ctrl Pts',(-33.5988578156673,2.36669353114775,310.59014149255));
#13212=CARTESIAN_POINT('Ctrl Pts',(-33.5492963636181,2.36281580961202,310.586850762041));
#13213=CARTESIAN_POINT('Ctrl Pts',(-33.5274929867878,2.36080577219749,310.585392078989));
#13214=CARTESIAN_POINT('Ctrl Pts',(-33.480504217366,2.35581688450475,310.58222318753));
#13215=CARTESIAN_POINT('Ctrl Pts',(-33.4553327154184,2.35273539131512,310.580509905376));
#13216=CARTESIAN_POINT('Ctrl Pts',(-33.385985087246,2.34311482008521,310.575744184977));
#13217=CARTESIAN_POINT('Ctrl Pts',(-33.3419387945491,2.33573109690969,310.572665693933));
#13218=CARTESIAN_POINT('Ctrl Pts',(-33.1206453953002,2.29217842944934,310.5569292862));
#13219=CARTESIAN_POINT('Ctrl Pts',(-32.9477635913037,2.23706217026844,310.543689705198));
#13220=CARTESIAN_POINT('Ctrl Pts',(-32.7447408112159,2.14570340258205,310.527456132776));
#13221=CARTESIAN_POINT('Ctrl Pts',(-32.7070915797467,2.12754985697098,310.524417945537));
#13222=CARTESIAN_POINT('Ctrl Pts',(-32.6699490276577,2.10841538128279,310.521403445152));
#13223=CARTESIAN_POINT('Ctrl Pts',(-32.6699491957805,2.10841546789345,310.326187962698));
#13224=CARTESIAN_POINT('Ctrl Pts',(-32.7011651547407,2.12449677779882,310.328752374967));
#13225=CARTESIAN_POINT('Ctrl Pts',(-32.7327438450632,2.13988772362731,310.331315189771));
#13226=CARTESIAN_POINT('Ctrl Pts',(-32.8407968834382,2.18961015778526,310.339959090314));
#13227=CARTESIAN_POINT('Ctrl Pts',(-32.9187427467795,2.2205882806106,310.345987861254));
#13228=CARTESIAN_POINT('Ctrl Pts',(-33.0181583841927,2.25411739408484,310.353298628881));
#13229=CARTESIAN_POINT('Ctrl Pts',(-33.0382343955691,2.26059133674271,310.354756052346));
#13230=CARTESIAN_POINT('Ctrl Pts',(-33.0710297139317,2.27068590917734,310.357103245601));
#13231=CARTESIAN_POINT('Ctrl Pts',(-33.0836972328514,2.27446939410077,310.358001793112));
#13232=CARTESIAN_POINT('Ctrl Pts',(-33.109357742748,2.28190044662387,310.359804769643));
#13233=CARTESIAN_POINT('Ctrl Pts',(-33.1223514830096,2.28554342286929,310.360708933401));
#13234=CARTESIAN_POINT('Ctrl Pts',(-33.1569891127496,2.2949364484048,310.363097553758));
#13235=CARTESIAN_POINT('Ctrl Pts',(-33.1786851174518,2.30049135490378,310.364571379883));
#13236=CARTESIAN_POINT('Ctrl Pts',(-33.3209219379867,2.33476959987433,310.3741079119));
#13237=CARTESIAN_POINT('Ctrl Pts',(-33.4434925666836,2.35431946690266,310.381744712001));
#13238=CARTESIAN_POINT('Ctrl Pts',(-33.6838307343132,2.37354121205113,310.396535475821));
#13239=CARTESIAN_POINT('Ctrl Pts',(-33.8011445154506,2.37421491980774,310.403674663504));
#13240=CARTESIAN_POINT('Ctrl Pts',(-33.989033200692,2.36135946997745,310.415473373532));
#13241=CARTESIAN_POINT('Ctrl Pts',(-34.0597808871005,2.35330761298922,310.419997967251));
#13242=CARTESIAN_POINT('Ctrl Pts',(-34.1592111274655,2.33743299786717,310.426537674418));
#13243=CARTESIAN_POINT('Ctrl Pts',(-34.1882766951603,2.3322341965814,310.428471281707));
#13244=CARTESIAN_POINT('Ctrl Pts',(-34.239087638206,2.3221635025539,310.431894057213));
#13245=CARTESIAN_POINT('Ctrl Pts',(-34.2608759030105,2.31752514523289,310.43337562169));
#13246=CARTESIAN_POINT('Ctrl Pts',(-34.3064457169066,2.30715100055669,310.436504987604));
#13247=CARTESIAN_POINT('Ctrl Pts',(-34.3302102099487,2.30135282402204,310.43815464441));
#13248=CARTESIAN_POINT('Ctrl Pts',(-34.3938992285348,2.28476581835318,310.442625478366));
#13249=CARTESIAN_POINT('Ctrl Pts',(-34.4336366568528,2.27329904631556,310.445468144841));
#13250=CARTESIAN_POINT('Ctrl Pts',(-34.6644297296454,2.20011198467773,310.462301201178));
#13251=CARTESIAN_POINT('Ctrl Pts',(-34.8473012037357,2.11537641930732,310.477049787446));
#13252=CARTESIAN_POINT('Ctrl Pts',(-35.0681994526253,1.97668396422446,310.496026389641));
#13253=CARTESIAN_POINT('Ctrl Pts',(-35.1178919759337,1.94278424111017,310.500373170706));
#13254=CARTESIAN_POINT('Ctrl Pts',(-35.1975278676907,1.88389898116342,310.50741264381));
#13255=CARTESIAN_POINT('Ctrl Pts',(-35.2282391506601,1.85999947978935,310.510146403672));
#13256=CARTESIAN_POINT('Ctrl Pts',(-35.2711866912039,1.82484723277534,310.513981370183));
#13257=CARTESIAN_POINT('Ctrl Pts',(-35.2839128079579,1.81420612297897,310.515119286153));
#13258=CARTESIAN_POINT('Ctrl Pts',(-35.3051380561325,1.79607659807025,310.517018281238));
#13259=CARTESIAN_POINT('Ctrl Pts',(-35.3136967150599,1.78865955423097,310.517784268625));
#13260=CARTESIAN_POINT('Ctrl Pts',(-35.3334030914736,1.77133303173797,310.519548362446));
#13261=CARTESIAN_POINT('Ctrl Pts',(-35.3445109323848,1.76137931508517,310.520543200644));
#13262=CARTESIAN_POINT('Ctrl Pts',(-35.3772002035143,1.73152577397186,310.523474981431));
#13263=CARTESIAN_POINT('Ctrl Pts',(-35.3985077335048,1.71132859336754,310.525391338802));
#13264=CARTESIAN_POINT('Ctrl Pts',(-35.5655155115799,1.54703039420045,310.540509236142));
#13265=CARTESIAN_POINT('Ctrl Pts',(-35.6923717339977,1.38497942603709,310.552662713756));
#13266=CARTESIAN_POINT('Ctrl Pts',(-35.8426623924278,1.13122049304195,310.570970407338));
#13267=CARTESIAN_POINT('Ctrl Pts',(-35.8840569167221,1.05128560280513,310.576637715341));
#13268=CARTESIAN_POINT('Ctrl Pts',(-35.9337821107498,0.940225575741763,
310.584516362532));
#13269=CARTESIAN_POINT('Ctrl Pts',(-35.9461709236824,0.910995812467881,
310.586589911926));
#13270=CARTESIAN_POINT('Ctrl Pts',(-35.9663734723491,0.860534735303168,
310.590174585424));
#13271=CARTESIAN_POINT('Ctrl Pts',(-35.9744771348981,0.839423682258381,
310.591675728817));
#13272=CARTESIAN_POINT('Ctrl Pts',(-35.989457869753,0.79866427695291,310.594578335277));
#13273=CARTESIAN_POINT('Ctrl Pts',(-35.9963805706928,0.779034846686049,
310.59597810656));
#13274=CARTESIAN_POINT('Ctrl Pts',(-36.014110658502,0.726569259143648,310.5997257169));
#13275=CARTESIAN_POINT('Ctrl Pts',(-36.0244596740544,0.693584710690194,
310.602088360564));
#13276=CARTESIAN_POINT('Ctrl Pts',(-36.0695957214243,0.537891271594074,
310.613277026865));
#13277=CARTESIAN_POINT('Ctrl Pts',(-36.095163840843,0.412749445140688,310.622391794552));
#13278=CARTESIAN_POINT('Ctrl Pts',(-36.1221584435765,0.190660779698225,
310.638652919245));
#13279=CARTESIAN_POINT('Ctrl Pts',(-36.127945006094,0.0945276924360876,
310.645714167013));
#13280=CARTESIAN_POINT('Ctrl Pts',(-36.127820176964,-0.0806002356389265,
310.658426354757));
#13281=CARTESIAN_POINT('Ctrl Pts',(-36.1238258690541,-0.159466075687365,
310.664093559647));
#13282=CARTESIAN_POINT('Ctrl Pts',(-36.113775825447,-0.259115622435795,
310.671073991351));
#13283=CARTESIAN_POINT('Ctrl Pts',(-36.1113619065198,-0.280209750604536,
310.672541201763));
#13284=CARTESIAN_POINT('Ctrl Pts',(-36.1071481372164,-0.313114014761444,
310.674810657776));
#13285=CARTESIAN_POINT('Ctrl Pts',(-36.1055418423012,-0.324947208666862,
310.67562291337));
#13286=CARTESIAN_POINT('Ctrl Pts',(-36.1019855680653,-0.349739145417503,
310.677315793509));
#13287=CARTESIAN_POINT('Ctrl Pts',(-36.1000174415893,-0.362694777831795,
310.678195274048));
#13288=CARTESIAN_POINT('Ctrl Pts',(-36.0946919369852,-0.39589559677855,
310.680437293506));
#13289=CARTESIAN_POINT('Ctrl Pts',(-36.0911789053681,-0.416115318425081,
310.681791446722));
#13290=CARTESIAN_POINT('Ctrl Pts',(-36.073634358068,-0.50986352787359,310.68802824569));
#13291=CARTESIAN_POINT('Ctrl Pts',(-36.0563881264073,-0.582753977717598,
310.692758356123));
#13292=CARTESIAN_POINT('Ctrl Pts',(-35.9842428490252,-0.833950872259935,
310.709020862149));
#13293=CARTESIAN_POINT('Ctrl Pts',(-35.9118074477784,-1.00648822683653,
310.720174099892));
#13294=CARTESIAN_POINT('Ctrl Pts',(-35.7905839553706,-1.2205425411179,310.735698819306));
#13295=CARTESIAN_POINT('Ctrl Pts',(-35.7593238002128,-1.2711966317769,310.739505601598));
#13296=CARTESIAN_POINT('Ctrl Pts',(-35.7107269612745,-1.34369221357061,
310.745189809146));
#13297=CARTESIAN_POINT('Ctrl Pts',(-35.6948562992226,-1.36649126204861,
310.747013234048));
#13298=CARTESIAN_POINT('Ctrl Pts',(-35.6656508373592,-1.40691327633599,
310.750314432869));
#13299=CARTESIAN_POINT('Ctrl Pts',(-35.6524630644113,-1.424638805468,310.75178641817));
#13300=CARTESIAN_POINT('Ctrl Pts',(-35.6235481638065,-1.46239003212115,
310.754975912167));
#13301=CARTESIAN_POINT('Ctrl Pts',(-35.6077424310716,-1.48235171786822,
310.756696422019));
#13302=CARTESIAN_POINT('Ctrl Pts',(-35.5621913481358,-1.53801457702003,
310.761593465543));
#13303=CARTESIAN_POINT('Ctrl Pts',(-35.5317152852311,-1.57309980086646,
310.764799148994));
#13304=CARTESIAN_POINT('Ctrl Pts',(-35.4349289253846,-1.67812627068785,
310.774775494571));
#13305=CARTESIAN_POINT('Ctrl Pts',(-35.3653770303368,-1.74493389484704,
310.781672246029));
#13306=CARTESIAN_POINT('Ctrl Pts',(-35.1615873884098,-1.91811143424261,
310.801072519459));
#13307=CARTESIAN_POINT('Ctrl Pts',(-35.019606062074,-2.01447126675836,310.813749277259));
#13308=CARTESIAN_POINT('Ctrl Pts',(-34.8433151022023,-2.10808743869885,
310.827795331842));
#13309=CARTESIAN_POINT('Ctrl Pts',(-34.817899766245,-2.12100197762021,310.829781260168));
#13310=CARTESIAN_POINT('Ctrl Pts',(-34.7789892724057,-2.13989916102562,
310.832756291068));
#13311=CARTESIAN_POINT('Ctrl Pts',(-34.7656618557438,-2.14621877987346,
310.833763845253));
#13312=CARTESIAN_POINT('Ctrl Pts',(-34.7408176422288,-2.15771681752271,
310.8356197602));
#13313=CARTESIAN_POINT('Ctrl Pts',(-34.7293177098188,-2.16292796360799,
310.836469921439));
#13314=CARTESIAN_POINT('Ctrl Pts',(-34.7015809405718,-2.17523075422512,
310.838499911205));
#13315=CARTESIAN_POINT('Ctrl Pts',(-34.6853053822581,-2.18223270263717,
310.839674446356));
#13316=CARTESIAN_POINT('Ctrl Pts',(-34.625880913126,-2.20701245170155,310.843908111494));
#13317=CARTESIAN_POINT('Ctrl Pts',(-34.5822854946532,-2.22369931324647,
310.846910102509));
#13318=CARTESIAN_POINT('Ctrl Pts',(-34.4627731646253,-2.26544399276511,
310.854934171966));
#13319=CARTESIAN_POINT('Ctrl Pts',(-34.3860345883638,-2.28796926376351,
310.85986757118));
#13320=CARTESIAN_POINT('Ctrl Pts',(-34.1370252069085,-2.34757984237678,
310.875589682449));
#13321=CARTESIAN_POINT('Ctrl Pts',(-33.9617335596669,-2.36937418315864,
310.886273625737));
#13322=CARTESIAN_POINT('Ctrl Pts',(-33.7473612677611,-2.37204290143076,
310.900047971212));
#13323=CARTESIAN_POINT('Ctrl Pts',(-33.7090678545138,-2.3715921934932,310.902533460109));
#13324=CARTESIAN_POINT('Ctrl Pts',(-33.646968098546,-2.3693567203049,310.90661374708));
#13325=CARTESIAN_POINT('Ctrl Pts',(-33.6231474633208,-2.36813920737541,
310.908190729571));
#13326=CARTESIAN_POINT('Ctrl Pts',(-33.5768980168004,-2.36507533214119,
310.911277567799));
#13327=CARTESIAN_POINT('Ctrl Pts',(-33.5544690833012,-2.36326857934525,
310.91278601397));
#13328=CARTESIAN_POINT('Ctrl Pts',(-33.501143218091,-2.35820830147416,310.916401293583));
#13329=CARTESIAN_POINT('Ctrl Pts',(-33.4702785328113,-2.35466634883782,
310.918516978761));
#13330=CARTESIAN_POINT('Ctrl Pts',(-33.3566789596785,-2.3393635915529,310.926393573988));
#13331=CARTESIAN_POINT('Ctrl Pts',(-33.2745212113791,-2.32384030791728,
310.93226922914));
#13332=CARTESIAN_POINT('Ctrl Pts',(-33.0339827305574,-2.26508779780068,
310.949988907547));
#13333=CARTESIAN_POINT('Ctrl Pts',(-32.8790771650479,-2.209726640577,310.962113087648));
#13334=CARTESIAN_POINT('Ctrl Pts',(-32.6723886202642,-2.11067621743435,
310.978668577832));
#13335=CARTESIAN_POINT('Ctrl Pts',(-32.6148131747072,-2.08010751403149,
310.983319138181));
#13336=CARTESIAN_POINT('Ctrl Pts',(-32.5411323121964,-2.03700608768373,
310.989258587811));
#13337=CARTESIAN_POINT('Ctrl Pts',(-32.5238298355319,-2.02658571479267,
310.990652386875));
#13338=CARTESIAN_POINT('Ctrl Pts',(-32.4966730155643,-2.00975415550389,
310.992835940888));
#13339=CARTESIAN_POINT('Ctrl Pts',(-32.4867300418211,-2.00348882745538,
310.993634532443));
#13340=CARTESIAN_POINT('Ctrl Pts',(-32.4656085456678,-1.9899592519621,310.995328383309));
#13341=CARTESIAN_POINT('Ctrl Pts',(-32.4544438005594,-1.98267409685331,
310.996222184687));
#13342=CARTESIAN_POINT('Ctrl Pts',(-32.4253323756866,-1.96332656665103,
310.998550269952));
#13343=CARTESIAN_POINT('Ctrl Pts',(-32.40748772637,-1.95111192151577,310.999974863183));
#13344=CARTESIAN_POINT('Ctrl Pts',(-32.3125122588902,-1.88417558564402,
311.007558220214));
#13345=CARTESIAN_POINT('Ctrl Pts',(-32.2385309434519,-1.82511573794859,
311.013471186566));
#13346=CARTESIAN_POINT('Ctrl Pts',(-32.0203684351065,-1.6284909033104,311.031601301038));
#13347=CARTESIAN_POINT('Ctrl Pts',(-31.8898539949585,-1.47711259938662,
311.043560579194));
#13348=CARTESIAN_POINT('Ctrl Pts',(-31.7583907698772,-1.2789626928131,311.058832140836));
#13349=CARTESIAN_POINT('Ctrl Pts',(-31.7377894573017,-1.24619777822806,
311.061343190847));
#13350=CARTESIAN_POINT('Ctrl Pts',(-31.7057605646045,-1.19237921389586,
311.06545460981));
#13351=CARTESIAN_POINT('Ctrl Pts',(-31.6938336881706,-1.17163003286189,
311.067036628468));
#13352=CARTESIAN_POINT('Ctrl Pts',(-31.6713242652929,-1.13106151461868,
311.070125841539));
#13353=CARTESIAN_POINT('Ctrl Pts',(-31.660705300896,-1.11126524047784,311.071631516382));
#13354=CARTESIAN_POINT('Ctrl Pts',(-31.6361833143755,-1.06394889052385,
311.075227703906));
#13355=CARTESIAN_POINT('Ctrl Pts',(-31.6225328856648,-1.03630327122741,
311.077326817044));
#13356=CARTESIAN_POINT('Ctrl Pts',(-31.5747733609412,-0.934631931756852,
311.085043173236));
#13357=CARTESIAN_POINT('Ctrl Pts',(-31.5439502570335,-0.85913442564733,
311.090768986721));
#13358=CARTESIAN_POINT('Ctrl Pts',(-31.4661520933852,-0.636439012895046,
311.10763293523));
#13359=CARTESIAN_POINT('Ctrl Pts',(-31.4295872613367,-0.486051380277261,
311.119014638653));
#13360=CARTESIAN_POINT('Ctrl Pts',(-31.3972455062377,-0.258120009955602,
311.135709129886));
#13361=CARTESIAN_POINT('Ctrl Pts',(-31.390198264663,-0.182568591936165,
311.141147620841));
#13362=CARTESIAN_POINT('Ctrl Pts',(-31.3858381534039,-0.0858425750154427,
311.147893260664));
#13363=CARTESIAN_POINT('Ctrl Pts',(-31.3851714666234,-0.0648698664965462,
311.149342818771));
#13364=CARTESIAN_POINT('Ctrl Pts',(-31.3845630456225,-0.0319974685479178,
311.151591564983));
#13365=CARTESIAN_POINT('Ctrl Pts',(-31.3844323916645,-0.0201029392975533,
311.152400476924));
#13366=CARTESIAN_POINT('Ctrl Pts',(-31.3843457119273,0.00494473858801117,
311.154093142395));
#13367=CARTESIAN_POINT('Ctrl Pts',(-31.3844096002821,0.0180974924238778,
311.154975679065));
#13368=CARTESIAN_POINT('Ctrl Pts',(-31.3848564556179,0.0520098164421929,
311.157236475168));
#13369=CARTESIAN_POINT('Ctrl Pts',(-31.3854026180852,0.0727667103384232,
311.158606067397));
#13370=CARTESIAN_POINT('Ctrl Pts',(-31.3893124398446,0.171851837503754,
311.165087652848));
#13371=CARTESIAN_POINT('Ctrl Pts',(-31.3962861721802,0.249996089538851,
311.170031963315));
#13372=CARTESIAN_POINT('Ctrl Pts',(-31.4205701688313,0.424089741716131,
311.180951287466));
#13373=CARTESIAN_POINT('Ctrl Pts',(-31.4399467155586,0.51960348412311,311.18687805144));
#13374=CARTESIAN_POINT('Ctrl Pts',(-31.4982013077625,0.737087040896473,
311.200703774959));
#13375=CARTESIAN_POINT('Ctrl Pts',(-31.5411791309906,0.857628214759107,
311.208625300651));
#13376=CARTESIAN_POINT('Ctrl Pts',(-31.6078586044818,1.0056527199718,311.219099460598));
#13377=CARTESIAN_POINT('Ctrl Pts',(-31.6227532956709,1.03687556162286,311.221352276305));
#13378=CARTESIAN_POINT('Ctrl Pts',(-31.6476971418992,1.08634933751992,311.22499864719));
#13379=CARTESIAN_POINT('Ctrl Pts',(-31.6573135209117,1.10481368720382,311.226377041321));
#13380=CARTESIAN_POINT('Ctrl Pts',(-31.6778781454419,1.14306204359842,311.229270511901));
#13381=CARTESIAN_POINT('Ctrl Pts',(-31.6888686917713,1.16282077861736,311.230786988676));
#13382=CARTESIAN_POINT('Ctrl Pts',(-31.7159563908558,1.20992081289204,311.234456117076));
#13383=CARTESIAN_POINT('Ctrl Pts',(-31.7323225958819,1.23710147205929,311.236618333008));
#13384=CARTESIAN_POINT('Ctrl Pts',(-31.7970653899712,1.33990046159224,311.244973876571));
#13385=CARTESIAN_POINT('Ctrl Pts',(-31.8491700621936,1.41307020866272,311.251301573704));
#13386=CARTESIAN_POINT('Ctrl Pts',(-32.0324343847769,1.64177456238361,311.272335707828));
#13387=CARTESIAN_POINT('Ctrl Pts',(-32.1794436600721,1.78342479607702,311.28750245237));
#13388=CARTESIAN_POINT('Ctrl Pts',(-32.3672230682471,1.92277810416287,311.303993761918));
#13389=CARTESIAN_POINT('Ctrl Pts',(-32.3920859383549,1.94049528944322,311.306124413192));
#13390=CARTESIAN_POINT('Ctrl Pts',(-32.4297803163327,1.96627353454686,311.309268611703));
#13391=CARTESIAN_POINT('Ctrl Pts',(-32.4423572675321,1.9746990301849,311.310303730107));
#13392=CARTESIAN_POINT('Ctrl Pts',(-32.4655134866528,1.98989257028258,311.312182920752));
#13393=CARTESIAN_POINT('Ctrl Pts',(-32.4760666611977,1.99669757921589,311.313029251201));
#13394=CARTESIAN_POINT('Ctrl Pts',(-32.5011110436123,2.01256678264139,311.315014619128));
#13395=CARTESIAN_POINT('Ctrl Pts',(-32.5156469133437,2.02155863227588,311.316149041684));
#13396=CARTESIAN_POINT('Ctrl Pts',(-32.5664109883932,2.05220739436852,311.320053804251));
#13397=CARTESIAN_POINT('Ctrl Pts',(-32.6031212099061,2.07305512132193,311.322778031315));
#13398=CARTESIAN_POINT('Ctrl Pts',(-32.6501942717952,2.09815031230247,311.326172696658));
#13399=CARTESIAN_POINT('Ctrl Pts',(-32.6600539326407,2.10331779286902,311.326878375156));
#13400=CARTESIAN_POINT('Ctrl Pts',(-32.6699490813724,2.10841540895464,311.327581625012));
#13401=CARTESIAN_POINT('Origin',(-33.7561270252576,0.,302.151410108095));
#13402=CARTESIAN_POINT('',(-32.6699490794746,2.10841540797695,312.522795280203));
#13403=CARTESIAN_POINT('',(-32.6699490794746,2.10841540797695,312.325750055738));
#13404=CARTESIAN_POINT('',(-32.6699490794746,2.10841540797695,302.151410108095));
#13405=CARTESIAN_POINT('',(-36.1275260743337,0.000498864453422136,311.848589849175));
#13406=CARTESIAN_POINT('Ctrl Pts',(-36.1278769729119,0.000498298962362804,
311.848589891905));
#13407=CARTESIAN_POINT('Ctrl Pts',(-36.127894235934,-0.081668381915641,
311.854074130266));
#13408=CARTESIAN_POINT('Ctrl Pts',(-36.1236373039452,-0.163782429335775,
311.859558368627));
#13409=CARTESIAN_POINT('Ctrl Pts',(-36.1151485915037,-0.245388085459784,
311.865042606987));
#13410=CARTESIAN_POINT('Ctrl Pts',(-36.1062342578652,-0.331085421834301,
311.870801823222));
#13411=CARTESIAN_POINT('Ctrl Pts',(-36.0926527766679,-0.416221524668992,
311.876561039456));
#13412=CARTESIAN_POINT('Ctrl Pts',(-36.0745139142165,-0.500280217081753,
311.88232025569));
#13413=CARTESIAN_POINT('Ctrl Pts',(-36.0571874318221,-0.580574196822511,
311.88782153555));
#13414=CARTESIAN_POINT('Ctrl Pts',(-36.0357032078721,-0.659884812496487,
311.89332281541));
#13415=CARTESIAN_POINT('Ctrl Pts',(-36.0102078988994,-0.737778745683441,
311.898824095271));
#13416=CARTESIAN_POINT('Ctrl Pts',(-35.9846821853252,-0.815765571801945,
311.904331935719));
#13417=CARTESIAN_POINT('Ctrl Pts',(-35.9551360074727,-0.892331954147945,
311.909839776167));
#13418=CARTESIAN_POINT('Ctrl Pts',(-35.9217638730913,-0.967065202457874,
311.915347616615));
#13419=CARTESIAN_POINT('Ctrl Pts',(-35.8883222260357,-1.04195411680592,
311.920866929651));
#13420=CARTESIAN_POINT('Ctrl Pts',(-35.8510389023304,-1.11500189615293,
311.926386242686));
#13421=CARTESIAN_POINT('Ctrl Pts',(-35.8101539097133,-1.18582107437559,
311.931905555721));
#13422=CARTESIAN_POINT('Ctrl Pts',(-35.8046040044569,-1.19543437510799,
311.932654771081));
#13423=CARTESIAN_POINT('Ctrl Pts',(-35.7989877963167,-1.2050066569793,311.93340398644));
#13424=CARTESIAN_POINT('Ctrl Pts',(-35.7933059444162,-1.21453699566369,
311.934153201799));
#13425=CARTESIAN_POINT('Ctrl Pts',(-35.7528702987077,-1.2823609033043,311.939485091357));
#13426=CARTESIAN_POINT('Ctrl Pts',(-35.708967236505,-1.3482917795089,311.944816980916));
#13427=CARTESIAN_POINT('Ctrl Pts',(-35.6617993488414,-1.41195292330395,
311.950148870474));
#13428=CARTESIAN_POINT('Ctrl Pts',(-35.6146996891026,-1.47552198182783,
311.955473047503));
#13429=CARTESIAN_POINT('Ctrl Pts',(-35.5643448589644,-1.53682745428348,
311.960797224531));
#13430=CARTESIAN_POINT('Ctrl Pts',(-35.5109821719493,-1.59551918717068,
311.966121401559));
#13431=CARTESIAN_POINT('Ctrl Pts',(-35.4576816657471,-1.65414252958002,
311.971439374596));
#13432=CARTESIAN_POINT('Ctrl Pts',(-35.4013805814392,-1.71015783971322,
311.976757347633));
#13433=CARTESIAN_POINT('Ctrl Pts',(-35.3423672253538,-1.76324703036719,
311.98207532067));
#13434=CARTESIAN_POINT('Ctrl Pts',(-35.2833915279335,-1.81630234279122,
311.987389900106));
#13435=CARTESIAN_POINT('Ctrl Pts',(-35.2217073416918,-1.86643492922096,
311.992704479542));
#13436=CARTESIAN_POINT('Ctrl Pts',(-35.1576397857835,-1.91336354219033,
311.998019058978));
#13437=CARTESIAN_POINT('Ctrl Pts',(-35.0935931520858,-1.96027682992512,
312.003331902859));
#13438=CARTESIAN_POINT('Ctrl Pts',(-35.0271650721852,-2.00398794501738,
312.008644746741));
#13439=CARTESIAN_POINT('Ctrl Pts',(-34.9587125253792,-2.04425687656842,
312.013957590622));
#13440=CARTESIAN_POINT('Ctrl Pts',(-34.8902610052486,-2.08452520415186,
312.01927035482));
#13441=CARTESIAN_POINT('Ctrl Pts',(-34.8197854833435,-2.12135121424258,
312.024583119017));
#13442=CARTESIAN_POINT('Ctrl Pts',(-34.747669314551,-2.15453984670573,312.029895883215));
#13443=CARTESIAN_POINT('Ctrl Pts',(-34.6754811747129,-2.18776160101411,
312.035213949485));
#13444=CARTESIAN_POINT('Ctrl Pts',(-34.6016495440834,-2.21733852968924,
312.040532015756));
#13445=CARTESIAN_POINT('Ctrl Pts',(-34.5265790874744,-2.24312319820511,
312.045850082026));
#13446=CARTESIAN_POINT('Ctrl Pts',(-34.4514726811573,-2.26892021447198,
312.05117069501));
#13447=CARTESIAN_POINT('Ctrl Pts',(-34.3751267181411,-2.29092122274619,
312.056491307994));
#13448=CARTESIAN_POINT('Ctrl Pts',(-34.2979599335368,-2.30902905178901,
312.061811920978));
#13449=CARTESIAN_POINT('Ctrl Pts',(-34.2206523851189,-2.3271699122337,312.067142239559));
#13450=CARTESIAN_POINT('Ctrl Pts',(-34.1425214855963,-2.34140331815997,
312.072472558141));
#13451=CARTESIAN_POINT('Ctrl Pts',(-34.0639948541079,-2.35168353790619,
312.077802876723));
#13452=CARTESIAN_POINT('Ctrl Pts',(-33.9890497781242,-2.36149488261062,
312.082890082471));
#13453=CARTESIAN_POINT('Ctrl Pts',(-33.9137446419557,-2.36770579685038,
312.08797728822));
#13454=CARTESIAN_POINT('Ctrl Pts',(-33.8384508664992,-2.3703208322215,312.093064493968));
#13455=CARTESIAN_POINT('Ctrl Pts',(-33.7595355956675,-2.37306164609749,
312.098396385177));
#13456=CARTESIAN_POINT('Ctrl Pts',(-33.6803337729824,-2.37186234919343,
312.103728276385));
#13457=CARTESIAN_POINT('Ctrl Pts',(-33.6012717911821,-2.3666892316017,312.109060167594));
#13458=CARTESIAN_POINT('Ctrl Pts',(-33.522324169655,-2.36152359673589,312.114384346416));
#13459=CARTESIAN_POINT('Ctrl Pts',(-33.4435164512169,-2.3523955862334,312.119708525239));
#13460=CARTESIAN_POINT('Ctrl Pts',(-33.3652769327858,-2.33932346367807,
312.125032704061));
#13461=CARTESIAN_POINT('Ctrl Pts',(-33.2871285798085,-2.32626657288809,
312.130350679098));
#13462=CARTESIAN_POINT('Ctrl Pts',(-33.2095475711884,-2.30927477960603,
312.135668654135));
#13463=CARTESIAN_POINT('Ctrl Pts',(-33.1329574487279,-2.28841817450127,
312.140986629173));
#13464=CARTESIAN_POINT('Ctrl Pts',(-33.0564161995297,-2.26757487829723,
312.146301210733));
#13465=CARTESIAN_POINT('Ctrl Pts',(-32.9808650326342,-2.24287178808603,
312.151615792294));
#13466=CARTESIAN_POINT('Ctrl Pts',(-32.9067164581259,-2.21442989298486,
312.156930373854));
#13467=CARTESIAN_POINT('Ctrl Pts',(-32.8325920962496,-2.18599728536019,
312.16224321998));
#13468=CARTESIAN_POINT('Ctrl Pts',(-32.7598698547046,-2.15382846492925,
312.167556066106));
#13469=CARTESIAN_POINT('Ctrl Pts',(-32.6889448333807,-2.1180935370849,312.172868912231));
#13470=CARTESIAN_POINT('Ctrl Pts',(-32.618020874264,-2.08235914442396,312.178181678789));
#13471=CARTESIAN_POINT('Ctrl Pts',(-32.5488944999614,-2.04305896265678,
312.183494445347));
#13472=CARTESIAN_POINT('Ctrl Pts',(-32.4819373074894,-2.00040961446246,
312.188807211906));
#13473=CARTESIAN_POINT('Ctrl Pts',(-32.4149132905271,-1.95771770144649,
312.194125280701));
#13474=CARTESIAN_POINT('Ctrl Pts',(-32.3500631764176,-1.91167019732476,
312.199443349496));
#13475=CARTESIAN_POINT('Ctrl Pts',(-32.2877300672236,-1.86252743231786,
312.204761418291));
#13476=CARTESIAN_POINT('Ctrl Pts',(-32.2253671068937,-1.81336113299066,
312.210082033894));
#13477=CARTESIAN_POINT('Ctrl Pts',(-32.1655239064085,-1.76109692860741,
312.215402649496));
#13478=CARTESIAN_POINT('Ctrl Pts',(-32.108508934623,-1.70603419951466,312.220723265098));
#13479=CARTESIAN_POINT('Ctrl Pts',(-32.0513899576581,-1.65087102647119,
312.226053586424));
#13480=CARTESIAN_POINT('Ctrl Pts',(-31.9971098399933,-1.59289947081792,
312.23138390775));
#13481=CARTESIAN_POINT('Ctrl Pts',(-31.9459386196224,-1.53245424029687,
312.236714229077));
#13482=CARTESIAN_POINT('Ctrl Pts',(-31.8971015075738,-1.47476613994748,
312.241801414764));
#13483=CARTESIAN_POINT('Ctrl Pts',(-31.8510960450867,-1.41482542098347,
312.246888600451));
#13484=CARTESIAN_POINT('Ctrl Pts',(-31.8081195609236,-1.35294677700163,
312.251975786138));
#13485=CARTESIAN_POINT('Ctrl Pts',(-31.7630763027158,-1.28809233875003,
312.257307618718));
#13486=CARTESIAN_POINT('Ctrl Pts',(-31.7211899938245,-1.22086312288555,
312.262639451299));
#13487=CARTESIAN_POINT('Ctrl Pts',(-31.6827199018342,-1.15159930663276,
312.267971283879));
#13488=CARTESIAN_POINT('Ctrl Pts',(-31.6443054574035,-1.08243568151933,
312.273295403885));
#13489=CARTESIAN_POINT('Ctrl Pts',(-31.6092976422666,-1.01124370697533,
312.27861952389));
#13490=CARTESIAN_POINT('Ctrl Pts',(-31.5779130645903,-0.938393309894114,
312.283943643895));
#13491=CARTESIAN_POINT('Ctrl Pts',(-31.5465650569767,-0.865627799843034,
312.289261560109));
#13492=CARTESIAN_POINT('Ctrl Pts',(-31.5188320815638,-0.791208135782106,
312.294579476322));
#13493=CARTESIAN_POINT('Ctrl Pts',(-31.4948846034213,-0.715528316831581,
312.299897392535));
#13494=CARTESIAN_POINT('Ctrl Pts',(-31.4709524065829,-0.639896790495606,
312.305211915293));
#13495=CARTESIAN_POINT('Ctrl Pts',(-31.4508010535546,-0.563007151119864,
312.31052643805));
#13496=CARTESIAN_POINT('Ctrl Pts',(-31.4345522474832,-0.485271690604297,
312.315840960808));
#13497=CARTESIAN_POINT('Ctrl Pts',(-31.418308747079,-0.407561612783178,
312.321153748233));
#13498=CARTESIAN_POINT('Ctrl Pts',(-31.4059653591345,-0.329006720823476,
312.326466535658));
#13499=CARTESIAN_POINT('Ctrl Pts',(-31.3975930684317,-0.250031272042916,
312.331779323083));
#13500=CARTESIAN_POINT('Ctrl Pts',(-31.3892209028309,-0.171057003342323,
312.337092031122));
#13501=CARTESIAN_POINT('Ctrl Pts',(-31.3848197646244,-0.091662656688382,
312.342404739161));
#13502=CARTESIAN_POINT('Ctrl Pts',(-31.3844088052639,-0.0122779253132078,
312.347717447201));
#13503=CARTESIAN_POINT('Ctrl Pts',(-31.3839974357001,0.0671860447643005,
312.353035458175));
#13504=CARTESIAN_POINT('Ctrl Pts',(-31.3875842036757,0.146639910430197,
312.35835346915));
#13505=CARTESIAN_POINT('Ctrl Pts',(-31.395136085621,0.225654260881445,312.363671480124));
#13506=CARTESIAN_POINT('Ctrl Pts',(-31.4026915845848,0.304706455722512,
312.368992038191));
#13507=CARTESIAN_POINT('Ctrl Pts',(-31.4142159127505,0.383318251454429,
312.374312596259));
#13508=CARTESIAN_POINT('Ctrl Pts',(-31.4296244623578,0.46106820246088,312.379633154326));
#13509=CARTESIAN_POINT('Ctrl Pts',(-31.4450611235255,0.53896000149998,312.384963419289));
#13510=CARTESIAN_POINT('Ctrl Pts',(-31.4643960521091,0.615986357909321,
312.390293684253));
#13511=CARTESIAN_POINT('Ctrl Pts',(-31.487494128881,0.691738999896711,312.395623949216));
#13512=CARTESIAN_POINT('Ctrl Pts',(-31.5095411209127,0.764044495750783,
312.400711658913));
#13513=CARTESIAN_POINT('Ctrl Pts',(-31.5350160632737,0.835189354047978,
312.40579936861));
#13514=CARTESIAN_POINT('Ctrl Pts',(-31.5637612271422,0.904837150958008,
312.410887078307));
#13515=CARTESIAN_POINT('Ctrl Pts',(-31.5938795252724,0.977811969297648,
312.416217823964));
#13516=CARTESIAN_POINT('Ctrl Pts',(-31.6277023981692,1.04941960203306,312.421548569621));
#13517=CARTESIAN_POINT('Ctrl Pts',(-31.665084385894,1.11925812164284,312.426879315278));
#13518=CARTESIAN_POINT('Ctrl Pts',(-31.7024162474512,1.18900299354797,312.432202912844));
#13519=CARTESIAN_POINT('Ctrl Pts',(-31.7432975322467,1.25698305129138,312.43752651041));
#13520=CARTESIAN_POINT('Ctrl Pts',(-31.7875346475331,1.32281597845853,312.442850107976));
#13521=CARTESIAN_POINT('Ctrl Pts',(-31.8317262322102,1.3885811477424,312.448168226282));
#13522=CARTESIAN_POINT('Ctrl Pts',(-31.8792665293994,1.45220318731645,312.453486344589));
#13523=CARTESIAN_POINT('Ctrl Pts',(-31.9299166404324,1.51332537573932,312.458804462895));
#13524=CARTESIAN_POINT('Ctrl Pts',(-31.9807043723432,1.5746136386101,312.464137031004));
#13525=CARTESIAN_POINT('Ctrl Pts',(-32.0346185914475,1.63338804235399,312.469469599113));
#13526=CARTESIAN_POINT('Ctrl Pts',(-32.0913757049304,1.68931971632635,312.474802167222));
#13527=CARTESIAN_POINT('Ctrl Pts',(-32.1479238672211,1.74504547796029,312.480115103493));
#13528=CARTESIAN_POINT('Ctrl Pts',(-32.2072936865423,1.79794907900351,312.485428039764));
#13529=CARTESIAN_POINT('Ctrl Pts',(-32.2691668342109,1.8477411757988,312.490740976035));
#13530=CARTESIAN_POINT('Ctrl Pts',(-32.331382923209,1.89780925286208,312.496083360063));
#13531=CARTESIAN_POINT('Ctrl Pts',(-32.3961298253543,1.94473090088057,312.501425744091));
#13532=CARTESIAN_POINT('Ctrl Pts',(-32.4630506189796,1.98825337168764,312.506768128119));
#13533=CARTESIAN_POINT('Ctrl Pts',(-32.529971412605,2.03177584249472,312.512110512147));
#13534=CARTESIAN_POINT('Ctrl Pts',(-32.5990656820435,2.07189889291044,312.517452896175));
#13535=CARTESIAN_POINT('Ctrl Pts',(-32.6699490794746,2.10841540797695,312.522795280203));
#13536=CARTESIAN_POINT('Ctrl Pts',(-32.671423404392,2.10551637491536,311.522951534327));
#13537=CARTESIAN_POINT('Ctrl Pts',(-33.0861637626343,2.31676127052873,311.554077895371));
#13538=CARTESIAN_POINT('Ctrl Pts',(-34.370461869201,2.57526687590523,311.638174687139));
#13539=CARTESIAN_POINT('Ctrl Pts',(-35.8730654168255,1.52349643505371,311.746720658333));
#13540=CARTESIAN_POINT('Ctrl Pts',(-36.124914683777,0.366246935917719,311.824140268482));
#13541=CARTESIAN_POINT('Ctrl Pts',(-36.1242308850569,0.000504174819979179,
311.848589447908));
#13542=CARTESIAN_POINT('',(-36.1278763296291,0.00181651129381628,311.651410108134));
#13543=CARTESIAN_POINT('Ctrl Pts',(-32.6699490813724,2.10841540895464,311.327581625012));
#13544=CARTESIAN_POINT('Ctrl Pts',(-32.7205654232083,2.13449108354362,311.331178936796));
#13545=CARTESIAN_POINT('Ctrl Pts',(-32.7721103252405,2.15873867404495,311.334712996911));
#13546=CARTESIAN_POINT('Ctrl Pts',(-32.9896249628738,2.25164825657492,311.349290190744));
#13547=CARTESIAN_POINT('Ctrl Pts',(-33.162230184724,2.30319960325097,311.360115343024));
#13548=CARTESIAN_POINT('Ctrl Pts',(-33.3839627058096,2.34281417314571,311.374477384485));
#13549=CARTESIAN_POINT('Ctrl Pts',(-33.4291487138416,2.34954661143632,311.377423744701));
#13550=CARTESIAN_POINT('Ctrl Pts',(-33.4998834845089,2.3580057069336,311.382082448808));
#13551=CARTESIAN_POINT('Ctrl Pts',(-33.5253148392667,2.36063070297005,311.383766632749));
#13552=CARTESIAN_POINT('Ctrl Pts',(-33.572782540978,2.36475590794514,311.38692985141));
#13553=CARTESIAN_POINT('Ctrl Pts',(-33.594807188374,2.36636040310828,311.388405424546));
#13554=CARTESIAN_POINT('Ctrl Pts',(-33.6444342595934,2.36927969869497,311.391749439544));
#13555=CARTESIAN_POINT('Ctrl Pts',(-33.6720432953709,2.37042008473026,311.39362315748));
#13556=CARTESIAN_POINT('Ctrl Pts',(-33.7582624873515,2.37247320724289,311.399518872214));
#13557=CARTESIAN_POINT('Ctrl Pts',(-33.8168867716744,2.37169578604935,311.403592168914));
#13558=CARTESIAN_POINT('Ctrl Pts',(-33.9601713987383,2.36447992657897,311.413709141659));
#13559=CARTESIAN_POINT('Ctrl Pts',(-34.0446273250634,2.355666506971,311.419812539606));
#13560=CARTESIAN_POINT('Ctrl Pts',(-34.2604796936735,2.32135866298747,311.4356949175));
#13561=CARTESIAN_POINT('Ctrl Pts',(-34.3905255546372,2.28923944315662,311.445548742057));
#13562=CARTESIAN_POINT('Ctrl Pts',(-34.5630680812351,2.23078289284199,311.458594258394));
#13563=CARTESIAN_POINT('Ctrl Pts',(-34.608479469465,2.21382976447803,311.462022857776));
#13564=CARTESIAN_POINT('Ctrl Pts',(-34.6703974044628,2.18852625533206,311.4666623385));
#13565=CARTESIAN_POINT('Ctrl Pts',(-34.6873708936482,2.18135792748381,311.467930379396));
#13566=CARTESIAN_POINT('Ctrl Pts',(-34.7159236097044,2.16890536913153,311.470054998019));
#13567=CARTESIAN_POINT('Ctrl Pts',(-34.7275467076526,2.16372452414726,311.470917434055));
#13568=CARTESIAN_POINT('Ctrl Pts',(-34.7522230155996,2.152486440578,311.472742602199));
#13569=CARTESIAN_POINT('Ctrl Pts',(-34.7652636258918,2.14640360766929,311.473703807661));
#13570=CARTESIAN_POINT('Ctrl Pts',(-34.8023373674329,2.12869786672292,311.476429183158));
#13571=CARTESIAN_POINT('Ctrl Pts',(-34.826231543144,2.11678698863427,311.478176889936));
#13572=CARTESIAN_POINT('Ctrl Pts',(-34.937685953362,2.05885892858413,311.486311244375));
#13573=CARTESIAN_POINT('Ctrl Pts',(-35.0225214041157,2.00779256912676,311.492452690073));
#13574=CARTESIAN_POINT('Ctrl Pts',(-35.260429073613,1.84348809778238,311.510239716022));
#13575=CARTESIAN_POINT('Ctrl Pts',(-35.4033468398871,1.71698387361544,311.521727117173));
#13576=CARTESIAN_POINT('Ctrl Pts',(-35.5537704365291,1.54757844631576,311.536313351547));
#13577=CARTESIAN_POINT('Ctrl Pts',(-35.5772895686174,1.5198314516041,311.538678107176));
#13578=CARTESIAN_POINT('Ctrl Pts',(-35.6149210354168,1.47330709005423,311.542611679588));
#13579=CARTESIAN_POINT('Ctrl Pts',(-35.6294094527706,1.45484082762781,311.544165125999));
#13580=CARTESIAN_POINT('Ctrl Pts',(-35.657375319916,1.41808636385474,311.547243666299));
#13581=CARTESIAN_POINT('Ctrl Pts',(-35.6708688087159,1.39981350674182,311.548767899338));
#13582=CARTESIAN_POINT('Ctrl Pts',(-35.7029329355317,1.35506114375053,311.552487425318));
#13583=CARTESIAN_POINT('Ctrl Pts',(-35.721227965454,1.32839078211471,311.554692955811));
#13584=CARTESIAN_POINT('Ctrl Pts',(-35.7917645191564,1.22091595110344,311.563541629351));
#13585=CARTESIAN_POINT('Ctrl Pts',(-35.8396073329563,1.137348394133,311.570341235822));
#13586=CARTESIAN_POINT('Ctrl Pts',(-35.9640172724249,0.885702064154583,
311.590544314634));
#13587=CARTESIAN_POINT('Ctrl Pts',(-36.0262080375081,0.711320133444521,
311.604257744596));
#13588=CARTESIAN_POINT('Ctrl Pts',(-36.0760279630006,0.494658036375356,
311.620044419309));
#13589=CARTESIAN_POINT('Ctrl Pts',(-36.0836175175372,0.457619193461639,
311.622698352683));
#13590=CARTESIAN_POINT('Ctrl Pts',(-36.0931971584312,0.404431606899662,
311.62643121419));
#13591=CARTESIAN_POINT('Ctrl Pts',(-36.0959113741356,0.388421125193596,
311.62754482376));
#13592=CARTESIAN_POINT('Ctrl Pts',(-36.1004261515361,0.360022666108016,
311.629500821265));
#13593=CARTESIAN_POINT('Ctrl Pts',(-36.1022933905915,0.347646548247032,
311.630346701726));
#13594=CARTESIAN_POINT('Ctrl Pts',(-36.10576382888,0.323341589605107,311.631995019574));
#13595=CARTESIAN_POINT('Ctrl Pts',(-36.107374296921,0.31141479668319,311.632797931021));
#13596=CARTESIAN_POINT('Ctrl Pts',(-36.1108662962818,0.283980671111723,
311.634632231051));
#13597=CARTESIAN_POINT('Ctrl Pts',(-36.1126855749867,0.268465804968367,
311.635660384521));
#13598=CARTESIAN_POINT('Ctrl Pts',(-36.1175734049914,0.222894162164295,
311.638656400295));
#13599=CARTESIAN_POINT('Ctrl Pts',(-36.1202212125426,0.192794368185148,
311.640604738208));
#13600=CARTESIAN_POINT('Ctrl Pts',(-36.1259712436791,0.109145623039551,
311.645955056815));
#13601=CARTESIAN_POINT('Ctrl Pts',(-36.1278334709158,0.0555286738497468,
311.649311870199));
#13602=CARTESIAN_POINT('Ctrl Pts',(-36.1278762701717,0.00189255109243725,
311.652636760053));
#13603=CARTESIAN_POINT('Ctrl Pts',(-36.1278763296291,0.00181651129381628,
311.651410108134));
#13604=CARTESIAN_POINT('Ctrl Pts',(-36.1279360242218,-0.0761244347127474,
311.65665745587));
#13605=CARTESIAN_POINT('Ctrl Pts',(-36.1241495396959,-0.154209488219651,
311.661904803605));
#13606=CARTESIAN_POINT('Ctrl Pts',(-36.1165007931509,-0.232020986854782,
311.667152151341));
#13607=CARTESIAN_POINT('Ctrl Pts',(-36.1088615680256,-0.309735623091775,
311.672392967));
#13608=CARTESIAN_POINT('Ctrl Pts',(-36.0973696750115,-0.387176902131175,
311.677633782659));
#13609=CARTESIAN_POINT('Ctrl Pts',(-36.0820610669041,-0.463927684461548,
311.682874598318));
#13610=CARTESIAN_POINT('Ctrl Pts',(-36.0667627704861,-0.540626768412813,
311.688111883828));
#13611=CARTESIAN_POINT('Ctrl Pts',(-36.0476529513995,-0.616635804913145,
311.693349169338));
#13612=CARTESIAN_POINT('Ctrl Pts',(-36.0248191594953,-0.691544693095099,
311.698586454848));
#13613=CARTESIAN_POINT('Ctrl Pts',(-36.0019931453665,-0.766428065387754,
311.703821956404));
#13614=CARTESIAN_POINT('Ctrl Pts',(-35.975445816364,-0.840211570422187,
311.709057457961));
#13615=CARTESIAN_POINT('Ctrl Pts',(-35.9453149843139,-0.912498845162449,
311.714292959517));
#13616=CARTESIAN_POINT('Ctrl Pts',(-35.9151843840198,-0.984785563893851,
311.719528420804));
#13617=CARTESIAN_POINT('Ctrl Pts',(-35.8814705237313,-1.05557562941191,
311.724763882091));
#13618=CARTESIAN_POINT('Ctrl Pts',(-35.8443592521434,-1.12449287640938,
311.729999343377));
#13619=CARTESIAN_POINT('Ctrl Pts',(-35.807211913622,-1.19347710127281,311.735239892796));
#13620=CARTESIAN_POINT('Ctrl Pts',(-35.766660803185,-1.26058444773637,311.740480442214));
#13621=CARTESIAN_POINT('Ctrl Pts',(-35.7229371941708,-1.32546437974002,
311.745720991632));
#13622=CARTESIAN_POINT('Ctrl Pts',(-35.6791906631924,-1.39037832484348,
311.750964288392));
#13623=CARTESIAN_POINT('Ctrl Pts',(-35.632268615843,-1.45306214577811,311.756207585152));
#13624=CARTESIAN_POINT('Ctrl Pts',(-35.582443414649,-1.51319744525969,311.761450881912));
#13625=CARTESIAN_POINT('Ctrl Pts',(-35.5325342744983,-1.57343405279763,
311.76670301189));
#13626=CARTESIAN_POINT('Ctrl Pts',(-35.4797125464819,-1.63111321409497,
311.771955141867));
#13627=CARTESIAN_POINT('Ctrl Pts',(-35.4242878302129,-1.68595302167966,
311.777207271845));
#13628=CARTESIAN_POINT('Ctrl Pts',(-35.3910604008471,-1.71882979499703,
311.780355953329));
#13629=CARTESIAN_POINT('Ctrl Pts',(-35.3568981046379,-1.75068684193181,
311.783504634813));
#13630=CARTESIAN_POINT('Ctrl Pts',(-35.3218729594151,-1.78147066553713,
311.786653316296));
#13631=CARTESIAN_POINT('Ctrl Pts',(-35.262562423286,-1.83359907415669,311.791985199596));
#13632=CARTESIAN_POINT('Ctrl Pts',(-35.2005333909952,-1.88286108117392,
311.797317082897));
#13633=CARTESIAN_POINT('Ctrl Pts',(-35.1360943489985,-1.92896040599787,
311.802648966197));
#13634=CARTESIAN_POINT('Ctrl Pts',(-35.0717485172144,-1.97499304876486,
311.807973136999));
#13635=CARTESIAN_POINT('Ctrl Pts',(-35.004999976621,-2.01787182371846,311.813297307801));
#13636=CARTESIAN_POINT('Ctrl Pts',(-34.9361916222065,-2.05733944927128,
311.818621478603));
#13637=CARTESIAN_POINT('Ctrl Pts',(-34.8674634457484,-2.09676108573469,
311.823939445491));
#13638=CARTESIAN_POINT('Ctrl Pts',(-34.796680629712,-2.13277923951948,311.829257412379));
#13639=CARTESIAN_POINT('Ctrl Pts',(-34.7242152333153,-2.16517973478409,
311.834575379267));
#13640=CARTESIAN_POINT('Ctrl Pts',(-34.6517960792214,-2.1975595543388,311.839889952604));
#13641=CARTESIAN_POINT('Ctrl Pts',(-34.5776969027343,-2.22632610655882,
311.845204525941));
#13642=CARTESIAN_POINT('Ctrl Pts',(-34.5023134833563,-2.25131158044595,
311.850519099277));
#13643=CARTESIAN_POINT('Ctrl Pts',(-34.4269546807666,-2.27628889521632,
311.855831937117));
#13644=CARTESIAN_POINT('Ctrl Pts',(-34.3503129127364,-2.29748743606748,
311.861144774956));
#13645=CARTESIAN_POINT('Ctrl Pts',(-34.2728016154043,-2.31478842022262,
311.866457612795));
#13646=CARTESIAN_POINT('Ctrl Pts',(-34.1952914796619,-2.33208914510403,
311.871770371016));
#13647=CARTESIAN_POINT('Ctrl Pts',(-34.1169122983884,-2.34549232855847,
311.877083129237));
#13648=CARTESIAN_POINT('Ctrl Pts',(-34.0380888041827,-2.35493006641926,
311.882395887457));
#13649=CARTESIAN_POINT('Ctrl Pts',(-33.9591866428774,-2.36437722329236,
311.887713947895));
#13650=CARTESIAN_POINT('Ctrl Pts',(-33.8798397494492,-2.36985097290238,
311.893032008333));
#13651=CARTESIAN_POINT('Ctrl Pts',(-33.8004785106302,-2.3713352795936,311.898350068771));
#13652=CARTESIAN_POINT('Ctrl Pts',(-33.721079266264,-2.37282029710901,311.903670675991));
#13653=CARTESIAN_POINT('Ctrl Pts',(-33.6416661320715,-2.3703120804766,311.908991283211));
#13654=CARTESIAN_POINT('Ctrl Pts',(-33.5626674490636,-2.36384674944863,
311.914311890431));
#13655=CARTESIAN_POINT('Ctrl Pts',(-33.4835246576759,-2.35736962444709,
311.919642203435));
#13656=CARTESIAN_POINT('Ctrl Pts',(-33.4047982942091,-2.34692102251696,
311.924972516438));
#13657=CARTESIAN_POINT('Ctrl Pts',(-33.3269093570692,-2.33258874553894,
311.930302829441));
#13658=CARTESIAN_POINT('Ctrl Pts',(-33.2525720247612,-2.31890999634082,
311.935390089116));
#13659=CARTESIAN_POINT('Ctrl Pts',(-33.1789977522611,-2.30169415298837,
311.940477348791));
#13660=CARTESIAN_POINT('Ctrl Pts',(-33.1065386255153,-2.28105961636696,
311.945564608466));
#13661=CARTESIAN_POINT('Ctrl Pts',(-33.030595253178,-2.25943285424569,311.950896492426));
#13662=CARTESIAN_POINT('Ctrl Pts',(-32.9555891915697,-2.23396839258137,
311.956228376386));
#13663=CARTESIAN_POINT('Ctrl Pts',(-32.8819365800715,-2.20476509588785,
311.961560260346));
#13664=CARTESIAN_POINT('Ctrl Pts',(-32.8083905058681,-2.17560404128413,
311.966884431824));
#13665=CARTESIAN_POINT('Ctrl Pts',(-32.7361944261268,-2.142715062857,311.972208603301));
#13666=CARTESIAN_POINT('Ctrl Pts',(-32.6657503312906,-2.10624707186824,
311.977532774779));
#13667=CARTESIAN_POINT('Ctrl Pts',(-32.5953883201663,-2.06982157454872,
311.982850742361));
#13668=CARTESIAN_POINT('Ctrl Pts',(-32.5267746513005,-2.02982556655169,
311.988168709944));
#13669=CARTESIAN_POINT('Ctrl Pts',(-32.4602908736375,-1.98645582147061,
311.993486677527));
#13670=CARTESIAN_POINT('Ctrl Pts',(-32.3938495210811,-1.9431137518033,311.99880125157));
#13671=CARTESIAN_POINT('Ctrl Pts',(-32.3295357536859,-1.89640247359618,
312.004115825612));
#13672=CARTESIAN_POINT('Ctrl Pts',(-32.2677049907753,-1.84656381145296,
312.009430399655));
#13673=CARTESIAN_POINT('Ctrl Pts',(-32.2058944188493,-1.79674142424491,
312.014743238211));
#13674=CARTESIAN_POINT('Ctrl Pts',(-32.1465656060824,-1.74379397501524,
312.020056076767));
#13675=CARTESIAN_POINT('Ctrl Pts',(-32.0900423192198,-1.68800468447423,
312.025368915323));
#13676=CARTESIAN_POINT('Ctrl Pts',(-32.0335198793195,-1.63221622989706,
312.03068167427));
#13677=CARTESIAN_POINT('Ctrl Pts',(-31.9798032145028,-1.57358634894655,
312.035994433216));
#13678=CARTESIAN_POINT('Ctrl Pts',(-31.9291794388162,-1.51243531395428,
312.041307192163));
#13679=CARTESIAN_POINT('Ctrl Pts',(-31.8785051397142,-1.45122324915724,
312.046625253336));
#13680=CARTESIAN_POINT('Ctrl Pts',(-31.8309301956454,-1.3874853659602,312.05194331451));
#13681=CARTESIAN_POINT('Ctrl Pts',(-31.7867011799799,-1.3215747812562,312.057261375683));
#13682=CARTESIAN_POINT('Ctrl Pts',(-31.7424509832956,-1.25563263235569,
312.062581983645));
#13683=CARTESIAN_POINT('Ctrl Pts',(-31.7015501488218,-1.18751611161875,
312.067902591607));
#13684=CARTESIAN_POINT('Ctrl Pts',(-31.6642002979126,-1.11760486305292,
312.073223199569));
#13685=CARTESIAN_POINT('Ctrl Pts',(-31.6267823138835,-1.0475660832824,312.078553513315));
#13686=CARTESIAN_POINT('Ctrl Pts',(-31.5929284577645,-0.975726458808749,
312.083883827062));
#13687=CARTESIAN_POINT('Ctrl Pts',(-31.5627929280154,-0.90248745164398,
312.089214140809));
#13688=CARTESIAN_POINT('Ctrl Pts',(-31.5340315680465,-0.832588117987969,
312.094301394084));
#13689=CARTESIAN_POINT('Ctrl Pts',(-31.5086568979712,-0.761414594229492,
312.09938864736));
#13690=CARTESIAN_POINT('Ctrl Pts',(-31.4867600707703,-0.689326982194133,
312.104475900635));
#13691=CARTESIAN_POINT('Ctrl Pts',(-31.4638103195706,-0.613772987745216,
312.109807777984));
#13692=CARTESIAN_POINT('Ctrl Pts',(-31.4445943310761,-0.536928478462323,
312.115139655332));
#13693=CARTESIAN_POINT('Ctrl Pts',(-31.4292543726937,-0.459196821907729,
312.120471532681));
#13694=CARTESIAN_POINT('Ctrl Pts',(-31.4139366033829,-0.381577603291414,
312.125795697531));
#13695=CARTESIAN_POINT('Ctrl Pts',(-31.4024838202053,-0.303074241846239,
312.131119862381));
#13696=CARTESIAN_POINT('Ctrl Pts',(-31.3949885562303,-0.224105315821012,
312.13644402723));
#13697=CARTESIAN_POINT('Ctrl Pts',(-31.3875020259773,-0.145228406921945,
312.141761988193));
#13698=CARTESIAN_POINT('Ctrl Pts',(-31.3839638950802,-0.0658874758163853,
312.147079949155));
#13699=CARTESIAN_POINT('Ctrl Pts',(-31.3844153905843,0.0134901614254798,
312.152397910117));
#13700=CARTESIAN_POINT('Ctrl Pts',(-31.384866597977,0.0928171456831942,
312.157712477547));
#13701=CARTESIAN_POINT('Ctrl Pts',(-31.3893023759705,0.172180322016819,
312.163027044977));
#13702=CARTESIAN_POINT('Ctrl Pts',(-31.3977119282638,0.251149940815805,
312.168341612406));
#13703=CARTESIAN_POINT('Ctrl Pts',(-31.4061187344199,0.330093772104531,
312.173654444365));
#13704=CARTESIAN_POINT('Ctrl Pts',(-31.4184966885462,0.408643835201987,
312.178967276324));
#13705=CARTESIAN_POINT('Ctrl Pts',(-31.4347830522822,0.486374569268121,
312.184280108283));
#13706=CARTESIAN_POINT('Ctrl Pts',(-31.4510691720554,0.564104138960999,
312.189592860658));
#13707=CARTESIAN_POINT('Ctrl Pts',(-31.4712634876137,0.641013945416478,
312.194905613033));
#13708=CARTESIAN_POINT('Ctrl Pts',(-31.495252262682,0.716689172827941,312.200218365408));
#13709=CARTESIAN_POINT('Ctrl Pts',(-31.5192649793855,0.792439926758653,
312.205536420096));
#13710=CARTESIAN_POINT('Ctrl Pts',(-31.5470795786416,0.866953192264275,
312.210854474783));
#13711=CARTESIAN_POINT('Ctrl Pts',(-31.5785327572063,0.939830445479384,
312.216172529471));
#13712=CARTESIAN_POINT('Ctrl Pts',(-31.6100009987479,1.01274259972627,312.221493130983));
#13713=CARTESIAN_POINT('Ctrl Pts',(-31.6451110835093,1.08401675969073,312.226813732495));
#13714=CARTESIAN_POINT('Ctrl Pts',(-31.6836530628696,1.15327782330353,312.232134334007));
#13715=CARTESIAN_POINT('Ctrl Pts',(-31.7222653511026,1.22266523401594,312.237464641443));
#13716=CARTESIAN_POINT('Ctrl Pts',(-31.7643217950518,1.29003181142169,312.242794948878));
#13717=CARTESIAN_POINT('Ctrl Pts',(-31.8095684211962,1.35503050277643,312.248125256314));
#13718=CARTESIAN_POINT('Ctrl Pts',(-31.8527523677748,1.41706606773059,312.253212568477));
#13719=CARTESIAN_POINT('Ctrl Pts',(-31.8988417181438,1.47694467569995,312.258299880641));
#13720=CARTESIAN_POINT('Ctrl Pts',(-31.9475831132455,1.53439466266794,312.263387192804));
#13721=CARTESIAN_POINT('Ctrl Pts',(-31.9986528195241,1.59458895858519,312.268717519058));
#13722=CARTESIAN_POINT('Ctrl Pts',(-32.0528277432143,1.65234484218041,312.274047845311));
#13723=CARTESIAN_POINT('Ctrl Pts',(-32.1098460819132,1.7073245497213,312.279378171564));
#13724=CARTESIAN_POINT('Ctrl Pts',(-32.1667924423372,1.76223485249541,312.284701768971));
#13725=CARTESIAN_POINT('Ctrl Pts',(-32.2265747624877,1.81437560954772,312.290025366377));
#13726=CARTESIAN_POINT('Ctrl Pts',(-32.2888913929784,1.86344242247249,312.295348963783));
#13727=CARTESIAN_POINT('Ctrl Pts',(-32.3511417192024,1.91245702880295,312.300666896935));
#13728=CARTESIAN_POINT('Ctrl Pts',(-32.4159206342127,1.95840389809495,312.305984830087));
#13729=CARTESIAN_POINT('Ctrl Pts',(-32.482891265758,2.00101693227009,312.31130276324));
#13730=CARTESIAN_POINT('Ctrl Pts',(-32.5435379039074,2.03960604520561,312.316118527406));
#13731=CARTESIAN_POINT('Ctrl Pts',(-32.6059812320803,2.07546152952587,312.320934291572));
#13732=CARTESIAN_POINT('Ctrl Pts',(-32.6699490794746,2.10841540797695,312.325750055738));
#13733=CARTESIAN_POINT('Origin',(-33.7561270252576,0.,302.151410108095));
#13734=CARTESIAN_POINT('',(-32.6699490794746,2.10841540797695,313.522886073942));
#13735=CARTESIAN_POINT('',(-32.669949079475,2.10841540797714,313.324578124683));
#13736=CARTESIAN_POINT('',(-32.6699490794746,2.10841540797695,302.151410108095));
#13737=CARTESIAN_POINT('',(-36.1278760162702,-0.0021877227769147,312.848589891943));
#13738=CARTESIAN_POINT('Ctrl Pts',(-36.1278760162702,-0.00218772277689684,
312.848589891943));
#13739=CARTESIAN_POINT('Ctrl Pts',(-36.1277803864196,-0.105861736697777,
312.85554583238));
#13740=CARTESIAN_POINT('Ctrl Pts',(-36.1208833294905,-0.209232213304625,
312.862501772816));
#13741=CARTESIAN_POINT('Ctrl Pts',(-36.1073257787753,-0.31154852584567,
312.869457713252));
#13742=CARTESIAN_POINT('Ctrl Pts',(-36.0955253581672,-0.400604104425696,
312.875512127106));
#13743=CARTESIAN_POINT('Ctrl Pts',(-36.078679841791,-0.488861716537749,
312.88156654096));
#13744=CARTESIAN_POINT('Ctrl Pts',(-36.0569106229126,-0.575841036451612,
312.887620954814));
#13745=CARTESIAN_POINT('Ctrl Pts',(-36.0377363360177,-0.652452257243405,
312.892953671108));
#13746=CARTESIAN_POINT('Ctrl Pts',(-36.0146951003667,-0.72824970273293,
312.898286387402));
#13747=CARTESIAN_POINT('Ctrl Pts',(-35.9878724107818,-0.80281417320027,
312.903619103696));
#13748=CARTESIAN_POINT('Ctrl Pts',(-35.9610885250329,-0.877270772774612,
312.908944105258));
#13749=CARTESIAN_POINT('Ctrl Pts',(-35.9305342065032,-0.950497502270844,
312.914269106821));
#13750=CARTESIAN_POINT('Ctrl Pts',(-35.8963454245516,-1.0220876996732,312.919594108383));
#13751=CARTESIAN_POINT('Ctrl Pts',(-35.8621965206471,-1.09359439374219,
312.924912898824));
#13752=CARTESIAN_POINT('Ctrl Pts',(-35.8244217786945,-1.16346792834909,
312.930231689266));
#13753=CARTESIAN_POINT('Ctrl Pts',(-35.7832056612843,-1.23132053741675,
312.935550479707));
#13754=CARTESIAN_POINT('Ctrl Pts',(-35.742015877669,-1.29912979410644,312.940865871868));
#13755=CARTESIAN_POINT('Ctrl Pts',(-35.6973893254698,-1.36492028861939,
312.946181264028));
#13756=CARTESIAN_POINT('Ctrl Pts',(-35.6495563344201,-1.42832892349921,
312.951496656189));
#13757=CARTESIAN_POINT('Ctrl Pts',(-35.6017390133426,-1.49171678586353,
312.95681030704));
#13758=CARTESIAN_POINT('Ctrl Pts',(-35.5507176213022,-1.55272396416407,
312.962123957891));
#13759=CARTESIAN_POINT('Ctrl Pts',(-35.4967648808627,-1.61101766537006,
312.967437608742));
#13760=CARTESIAN_POINT('Ctrl Pts',(-35.4428130188985,-1.66931041741987,
312.972751173075));
#13761=CARTESIAN_POINT('Ctrl Pts',(-35.3859302227345,-1.72488943713238,
312.978064737407));
#13762=CARTESIAN_POINT('Ctrl Pts',(-35.3264274278707,-1.77745737165566,
312.98337830174));
#13763=CARTESIAN_POINT('Ctrl Pts',(-35.2668654415753,-1.83007759903868,
312.988697151832));
#13764=CARTESIAN_POINT('Ctrl Pts',(-35.2046786022178,-1.87968044658249,
312.994016001924));
#13765=CARTESIAN_POINT('Ctrl Pts',(-35.1402119786694,-1.92600802289063,
312.999334852016));
#13766=CARTESIAN_POINT('Ctrl Pts',(-35.0757145801997,-1.97235771494546,
313.004656241208));
#13767=CARTESIAN_POINT('Ctrl Pts',(-35.0089356237967,-2.01542876648465,
313.009977630401));
#13768=CARTESIAN_POINT('Ctrl Pts',(-34.940248143378,-2.05500735768059,313.015299019593));
#13769=CARTESIAN_POINT('Ctrl Pts',(-34.8714356706571,-2.09465797101505,
313.020630092248));
#13770=CARTESIAN_POINT('Ctrl Pts',(-34.8007081524456,-2.13080321061484,
313.025961164903));
#13771=CARTESIAN_POINT('Ctrl Pts',(-34.7284619600125,-2.16327595030203,
313.031292237559));
#13772=CARTESIAN_POINT('Ctrl Pts',(-34.6596182378814,-2.19421937019132,
313.0363722407));
#13773=CARTESIAN_POINT('Ctrl Pts',(-34.5893960069771,-2.22182831486617,
313.041452243842));
#13774=CARTESIAN_POINT('Ctrl Pts',(-34.5181506453613,-2.24600045968474,
313.046532246984));
#13775=CARTESIAN_POINT('Ctrl Pts',(-34.4433707229326,-2.27137181121518,
313.051864274673));
#13776=CARTESIAN_POINT('Ctrl Pts',(-34.3671808330306,-2.29305242269349,
313.057196302363));
#13777=CARTESIAN_POINT('Ctrl Pts',(-34.2899796105284,-2.31088716290944,
313.062528330052));
#13778=CARTESIAN_POINT('Ctrl Pts',(-34.2128899123519,-2.32869613918914,
313.067852655133));
#13779=CARTESIAN_POINT('Ctrl Pts',(-34.1347922357811,-2.34267017248802,
313.073176980214));
#13780=CARTESIAN_POINT('Ctrl Pts',(-34.0561020108446,-2.35270335370231,
313.078501305295));
#13781=CARTESIAN_POINT('Ctrl Pts',(-33.9775032689726,-2.36272487061947,
313.083819440464));
#13782=CARTESIAN_POINT('Ctrl Pts',(-33.8983138103218,-2.36881458095319,
313.089137575632));
#13783=CARTESIAN_POINT('Ctrl Pts',(-33.8189594424695,-2.37091757550686,
313.094455710801));
#13784=CARTESIAN_POINT('Ctrl Pts',(-33.7396555858598,-2.37301923144652,
313.09977046083));
#13785=CARTESIAN_POINT('Ctrl Pts',(-33.6601874957708,-2.37113919603529,
313.10508521086));
#13786=CARTESIAN_POINT('Ctrl Pts',(-33.5809850785911,-2.36527447900193,
313.110399960889));
#13787=CARTESIAN_POINT('Ctrl Pts',(-33.5018084038412,-2.35941166812337,
313.115712983514));
#13788=CARTESIAN_POINT('Ctrl Pts',(-33.4228976977028,-2.34956678191858,
313.121026006139));
#13789=CARTESIAN_POINT('Ctrl Pts',(-33.3446803444295,-2.3357888798724,313.126339028764));
#13790=CARTESIAN_POINT('Ctrl Pts',(-33.2664640487071,-2.32201116411265,
313.131651979553));
#13791=CARTESIAN_POINT('Ctrl Pts',(-33.1889415486718,-2.30430062086182,
313.136964930343));
#13792=CARTESIAN_POINT('Ctrl Pts',(-33.1125311238695,-2.28275762581497,
313.142277881132));
#13793=CARTESIAN_POINT('Ctrl Pts',(-33.0360442884017,-2.26119308770524,
313.147596144889));
#13794=CARTESIAN_POINT('Ctrl Pts',(-32.96067220197,-2.23578856947746,313.152914408646));
#13795=CARTESIAN_POINT('Ctrl Pts',(-32.8868184508175,-2.2066945110062,313.158232672403));
#13796=CARTESIAN_POINT('Ctrl Pts',(-32.8129292469554,-2.17758648624088,
313.163553489136));
#13797=CARTESIAN_POINT('Ctrl Pts',(-32.7405602579407,-2.14478558668956,
313.168874305869));
#13798=CARTESIAN_POINT('Ctrl Pts',(-32.6700931563666,-2.10848962485513,
313.174195122602));
#13799=CARTESIAN_POINT('Ctrl Pts',(-32.5994974099785,-2.07212740107497,
313.179525653024));
#13800=CARTESIAN_POINT('Ctrl Pts',(-32.5308108956193,-2.03225760100031,
313.184856183446));
#13801=CARTESIAN_POINT('Ctrl Pts',(-32.4643886639911,-1.989122939522,313.190186713867));
#13802=CARTESIAN_POINT('Ctrl Pts',(-32.4010183360325,-1.9479701872392,313.195272322296));
#13803=CARTESIAN_POINT('Ctrl Pts',(-32.3397090541619,-1.90384624575719,
313.200357930725));
#13804=CARTESIAN_POINT('Ctrl Pts',(-32.280740185164,-1.85699535125395,313.205443539153));
#13805=CARTESIAN_POINT('Ctrl Pts',(-32.2189629243854,-1.80791318338083,
313.210771349631));
#13806=CARTESIAN_POINT('Ctrl Pts',(-32.1595194065857,-1.75565099827935,
313.216099160109));
#13807=CARTESIAN_POINT('Ctrl Pts',(-32.1027557233654,-1.70045917345262,
313.221426970587));
#13808=CARTESIAN_POINT('Ctrl Pts',(-32.0460743470137,-1.64534737631299,
313.226747055783));
#13809=CARTESIAN_POINT('Ctrl Pts',(-31.9920654229078,-1.58731469948817,
313.23206714098));
#13810=CARTESIAN_POINT('Ctrl Pts',(-31.9410428092489,-1.52665233478226,
313.237387226177));
#13811=CARTESIAN_POINT('Ctrl Pts',(-31.8900796960507,-1.46606071201581,
313.242701107311));
#13812=CARTESIAN_POINT('Ctrl Pts',(-31.8420962738445,-1.40284585266758,
313.248014988445));
#13813=CARTESIAN_POINT('Ctrl Pts',(-31.797369184335,-1.33733532934864,313.253328869578));
#13814=CARTESIAN_POINT('Ctrl Pts',(-31.7526706448738,-1.27186662249119,
313.258639358773));
#13815=CARTESIAN_POINT('Ctrl Pts',(-31.7112245768274,-1.20410554679715,
313.263949847968));
#13816=CARTESIAN_POINT('Ctrl Pts',(-31.6732662206456,-1.13441127070882,
313.269260337162));
#13817=CARTESIAN_POINT('Ctrl Pts',(-31.635320218597,-1.06473967769885,313.274569097976));
#13818=CARTESIAN_POINT('Ctrl Pts',(-31.6008598989647,-0.993136545736397,
313.27987785879));
#13819=CARTESIAN_POINT('Ctrl Pts',(-31.570075395045,-0.919987137162623,
313.285186619604));
#13820=CARTESIAN_POINT('Ctrl Pts',(-31.5392912796118,-0.846838651701281,
313.290495313423));
#13821=CARTESIAN_POINT('Ctrl Pts',(-31.512183068623,-0.772144361806512,
313.295804007243));
#13822=CARTESIAN_POINT('Ctrl Pts',(-31.4888928321102,-0.696309683921922,
313.301112701063));
#13823=CARTESIAN_POINT('Ctrl Pts',(-31.4655791217774,-0.620398573598213,
313.306426745422));
#13824=CARTESIAN_POINT('Ctrl Pts',(-31.4460912110809,-0.543345229299718,
313.311740789781));
#13825=CARTESIAN_POINT('Ctrl Pts',(-31.4305211288046,-0.465569841036638,
313.31705483414));
#13826=CARTESIAN_POINT('Ctrl Pts',(-31.4149435268195,-0.387756890463096,
313.322371444963));
#13827=CARTESIAN_POINT('Ctrl Pts',(-31.4032875914132,-0.309221666466385,
313.327688055787));
#13828=CARTESIAN_POINT('Ctrl Pts',(-31.3955936577933,-0.230391587493498,
313.33300466661));
#13829=CARTESIAN_POINT('Ctrl Pts',(-31.3878855610137,-0.151416396402887,
313.338331064366));
#13830=CARTESIAN_POINT('Ctrl Pts',(-31.3841540618197,-0.0721457361033145,
313.343657462122));
#13831=CARTESIAN_POINT('Ctrl Pts',(-31.3843873287825,0.00699104172302907,
313.348983859878));
#13832=CARTESIAN_POINT('Ctrl Pts',(-31.3846117168204,0.0831156076991083,
313.354107517027));
#13833=CARTESIAN_POINT('Ctrl Pts',(-31.3885044163401,0.159115927399626,
313.359231174175));
#13834=CARTESIAN_POINT('Ctrl Pts',(-31.3960098112352,0.234616279433132,
313.364354831323));
#13835=CARTESIAN_POINT('Ctrl Pts',(-31.4038328626931,0.313312090553255,
313.369695340927));
#13836=CARTESIAN_POINT('Ctrl Pts',(-31.4156108517525,0.391763030641342,
313.375035850532));
#13837=CARTESIAN_POINT('Ctrl Pts',(-31.4313196407786,0.469540932796829,
313.380376360136));
#13838=CARTESIAN_POINT('Ctrl Pts',(-31.4470056964146,0.547206276601627,
313.385709141081));
#13839=CARTESIAN_POINT('Ctrl Pts',(-31.4666111625597,0.624200062725887,
313.391041922025));
#13840=CARTESIAN_POINT('Ctrl Pts',(-31.4900601455345,0.700099249479816,
313.39637470297));
#13841=CARTESIAN_POINT('Ctrl Pts',(-31.513481539297,0.775909136037327,313.40170120956));
#13842=CARTESIAN_POINT('Ctrl Pts',(-31.5407373250942,0.850626538719343,
313.40702771615));
#13843=CARTESIAN_POINT('Ctrl Pts',(-31.571700895418,0.923840108338071,313.412354222741));
#13844=CARTESIAN_POINT('Ctrl Pts',(-31.6026444800451,0.997006421642888,
313.417677291292));
#13845=CARTESIAN_POINT('Ctrl Pts',(-31.6372909170154,1.06867039958483,313.423000359844));
#13846=CARTESIAN_POINT('Ctrl Pts',(-31.6754646407872,1.13843844996113,313.428323428396));
#13847=CARTESIAN_POINT('Ctrl Pts',(-31.7136255167986,1.20818301918062,313.433644705414));
#13848=CARTESIAN_POINT('Ctrl Pts',(-31.7553110979245,1.27603251853521,313.438965982433));
#13849=CARTESIAN_POINT('Ctrl Pts',(-31.8002994718418,1.34161717483033,313.444287259451));
#13850=CARTESIAN_POINT('Ctrl Pts',(-31.8452866008212,1.40720001623811,313.449608389216));
#13851=CARTESIAN_POINT('Ctrl Pts',(-31.8935760755625,1.47051775466638,313.454929518982));
#13852=CARTESIAN_POINT('Ctrl Pts',(-31.9449030141891,1.53123010819042,313.460250648747));
#13853=CARTESIAN_POINT('Ctrl Pts',(-31.9962791591546,1.59200066570493,313.465576879797));
#13854=CARTESIAN_POINT('Ctrl Pts',(-32.0506982828648,1.65016049104283,313.470903110847));
#13855=CARTESIAN_POINT('Ctrl Pts',(-32.1078559892727,1.70540337000759,313.476229341897));
#13856=CARTESIAN_POINT('Ctrl Pts',(-32.165040217359,1.76067188215399,313.481558044365));
#13857=CARTESIAN_POINT('Ctrl Pts',(-32.2249652078903,1.8130204431315,313.486886746833));
#13858=CARTESIAN_POINT('Ctrl Pts',(-32.2872924442793,1.86218233162658,313.492215449301));
#13859=CARTESIAN_POINT('Ctrl Pts',(-32.3497294374532,1.91143079304122,313.497553535488));
#13860=CARTESIAN_POINT('Ctrl Pts',(-32.4145767478216,1.95748109725601,313.502891621675));
#13861=CARTESIAN_POINT('Ctrl Pts',(-32.4814659584981,2.00010930386008,313.508229707861));
#13862=CARTESIAN_POINT('Ctrl Pts',(-32.5426834513249,2.0391229490445,313.513115163222));
#13863=CARTESIAN_POINT('Ctrl Pts',(-32.6056106806806,2.07527063509553,313.518000618582));
#13864=CARTESIAN_POINT('Ctrl Pts',(-32.6699490794746,2.10841540797695,313.522886073942));
#13865=CARTESIAN_POINT('Ctrl Pts',(-32.6699490794746,2.10841540797695,312.522795280203));
#13866=CARTESIAN_POINT('Ctrl Pts',(-32.7405450600518,2.14478385646856,312.528116002019));
#13867=CARTESIAN_POINT('Ctrl Pts',(-32.8129152355776,2.17757481367262,312.533436723835));
#13868=CARTESIAN_POINT('Ctrl Pts',(-32.8866592463607,2.20663178712718,312.538757445651));
#13869=CARTESIAN_POINT('Ctrl Pts',(-32.9605374302371,2.2357416281159,312.544087848221));
#13870=CARTESIAN_POINT('Ctrl Pts',(-33.035793998677,2.26110375999759,312.549418250792));
#13871=CARTESIAN_POINT('Ctrl Pts',(-33.1120124034452,2.28261131524128,312.554748653363));
#13872=CARTESIAN_POINT('Ctrl Pts',(-33.1837434103354,2.30285260208094,312.559765225734));
#13873=CARTESIAN_POINT('Ctrl Pts',(-33.2563258906175,2.31968023219454,312.564781798105));
#13874=CARTESIAN_POINT('Ctrl Pts',(-33.3294068249702,2.33304692048117,312.569798370476));
#13875=CARTESIAN_POINT('Ctrl Pts',(-33.4070818752241,2.34725388422061,312.575130301635));
#13876=CARTESIAN_POINT('Ctrl Pts',(-33.4856143465868,2.35760442458897,312.580462232795));
#13877=CARTESIAN_POINT('Ctrl Pts',(-33.5645872962858,2.36400308686884,312.585794163954));
#13878=CARTESIAN_POINT('Ctrl Pts',(-33.6434460292288,2.37039249491102,312.591118383664));
#13879=CARTESIAN_POINT('Ctrl Pts',(-33.7227435120484,2.37284133753259,312.596442603375));
#13880=CARTESIAN_POINT('Ctrl Pts',(-33.8020533484656,2.37130530200913,312.601766823085));
#13881=CARTESIAN_POINT('Ctrl Pts',(-33.8812707909413,2.36977105592796,312.607084840215));
#13882=CARTESIAN_POINT('Ctrl Pts',(-33.9605000921013,2.36426116596706,312.612402857344));
#13883=CARTESIAN_POINT('Ctrl Pts',(-34.0393120115705,2.35478328642509,312.617720874474));
#13884=CARTESIAN_POINT('Ctrl Pts',(-34.1180736509638,2.34531145353833,312.623035498839));
#13885=CARTESIAN_POINT('Ctrl Pts',(-34.1964179729635,2.33187671144784,312.628350123204));
#13886=CARTESIAN_POINT('Ctrl Pts',(-34.2739192380045,2.31453867691137,312.633664747569));
#13887=CARTESIAN_POINT('Ctrl Pts',(-34.351395205256,2.29720630181735,312.638977637146));
#13888=CARTESIAN_POINT('Ctrl Pts',(-34.4280282048192,2.27597326655007,312.644290526723));
#13889=CARTESIAN_POINT('Ctrl Pts',(-34.5034025678486,2.25095031618765,312.6496034163));
#13890=CARTESIAN_POINT('Ctrl Pts',(-34.5787758103104,2.22592773783379,312.654916226893));
#13891=CARTESIAN_POINT('Ctrl Pts',(-34.6528900089037,2.19711550536241,312.660229037485));
#13892=CARTESIAN_POINT('Ctrl Pts',(-34.725345971637,2.16467380833216,312.665541848077));
#13893=CARTESIAN_POINT('Ctrl Pts',(-34.7978742542544,2.13219973053319,312.670859961501));
#13894=CARTESIAN_POINT('Ctrl Pts',(-34.8687405657672,2.09608914348932,312.676178074926));
#13895=CARTESIAN_POINT('Ctrl Pts',(-34.9375675389942,2.056549628626,312.681496188351));
#13896=CARTESIAN_POINT('Ctrl Pts',(-35.0064274781194,2.01699117561153,312.68681684898));
#13897=CARTESIAN_POINT('Ctrl Pts',(-35.0732457382495,1.97400077698668,312.69213750961));
#13898=CARTESIAN_POINT('Ctrl Pts',(-35.1376735281126,1.92782969241295,312.697458170239));
#13899=CARTESIAN_POINT('Ctrl Pts',(-35.2022188459847,1.88157438338188,312.702788536721));
#13900=CARTESIAN_POINT('Ctrl Pts',(-35.2643646120948,1.83212708694795,312.708118903203));
#13901=CARTESIAN_POINT('Ctrl Pts',(-35.3237949104075,1.77977961117932,312.713449269686));
#13902=CARTESIAN_POINT('Ctrl Pts',(-35.3805095665181,1.72982413104941,312.718536067339));
#13903=CARTESIAN_POINT('Ctrl Pts',(-35.4347512701437,1.67722800610831,312.723622864992));
#13904=CARTESIAN_POINT('Ctrl Pts',(-35.486279014651,1.62227376114459,312.728709662645));
#13905=CARTESIAN_POINT('Ctrl Pts',(-35.5396271593962,1.56537806266751,312.733976169458));
#13906=CARTESIAN_POINT('Ctrl Pts',(-35.5902789241322,1.50572711898534,312.739242676271));
#13907=CARTESIAN_POINT('Ctrl Pts',(-35.6379314395801,1.44361013044951,312.744509183083));
#13908=CARTESIAN_POINT('Ctrl Pts',(-35.6855211242083,1.38157504443795,312.749768745899));
#13909=CARTESIAN_POINT('Ctrl Pts',(-35.7301191118534,1.31708073912948,312.755028308714));
#13910=CARTESIAN_POINT('Ctrl Pts',(-35.7714598544099,1.25045257816565,312.76028787153));
#13911=CARTESIAN_POINT('Ctrl Pts',(-35.8127597196738,1.18389029842842,312.765542233744));
#13912=CARTESIAN_POINT('Ctrl Pts',(-35.8508084769252,1.1151987550711,312.770796595959));
#13913=CARTESIAN_POINT('Ctrl Pts',(-35.8853823420327,1.04473434828417,312.776050958174));
#13914=CARTESIAN_POINT('Ctrl Pts',(-35.9199334147536,0.974316394273128,
312.781301856517));
#13915=CARTESIAN_POINT('Ctrl Pts',(-35.9510139310135,0.902128327428168,
312.786552754859));
#13916=CARTESIAN_POINT('Ctrl Pts',(-35.9784455896821,0.828551905866046,
312.791803653202));
#13917=CARTESIAN_POINT('Ctrl Pts',(-36.0058765309656,0.75497740845396,312.797054414224));
#13918=CARTESIAN_POINT('Ctrl Pts',(-36.0296586205228,0.680015073258473,
312.802305175247));
#13919=CARTESIAN_POINT('Ctrl Pts',(-36.0496618558139,0.604066257562219,
312.807555936269));
#13920=CARTESIAN_POINT('Ctrl Pts',(-36.069664292838,0.528120472747102,312.81280648775));
#13921=CARTESIAN_POINT('Ctrl Pts',(-36.0858880609003,0.451188753325259,
312.818057039231));
#13922=CARTESIAN_POINT('Ctrl Pts',(-36.0982537172768,0.373685189740282,
312.823307590712));
#13923=CARTESIAN_POINT('Ctrl Pts',(-36.1106293976277,0.296118799427103,
312.828562398448));
#13924=CARTESIAN_POINT('Ctrl Pts',(-36.1191406563015,0.217980116654933,
312.833817206185));
#13925=CARTESIAN_POINT('Ctrl Pts',(-36.1237597639975,0.139689931444203,
312.839072013921));
#13926=CARTESIAN_POINT('Ctrl Pts',(-36.1265485817589,0.0924216983950322,
312.842244639916));
#13927=CARTESIAN_POINT('Ctrl Pts',(-36.1279196333306,0.0450983169026677,
312.84541726591));
#13928=CARTESIAN_POINT('Ctrl Pts',(-36.1278760162707,-0.00218772220706814,
312.848589891905));
#13929=CARTESIAN_POINT('',(-36.1278769078432,0.000746294306655331,312.651410108059));
#13930=CARTESIAN_POINT('Ctrl Pts',(-32.6699490794746,2.10841540797695,312.325750055738));
#13931=CARTESIAN_POINT('Ctrl Pts',(-32.7405208763421,2.1447713979122,312.331062992539));
#13932=CARTESIAN_POINT('Ctrl Pts',(-32.812948244602,2.1775948627673,312.33637592934));
#13933=CARTESIAN_POINT('Ctrl Pts',(-32.8868415286018,2.20670360216407,312.341688866141));
#13934=CARTESIAN_POINT('Ctrl Pts',(-32.9607315335957,2.2358110498639,312.347001567181));
#13935=CARTESIAN_POINT('Ctrl Pts',(-33.0360868884612,2.26120392885337,312.352314268221));
#13936=CARTESIAN_POINT('Ctrl Pts',(-33.1124987676385,2.28274850311949,312.357626969261));
#13937=CARTESIAN_POINT('Ctrl Pts',(-33.1900122585412,2.30460368034269,312.363016262237));
#13938=CARTESIAN_POINT('Ctrl Pts',(-33.2686125083594,2.32249855389248,312.368405555214));
#13939=CARTESIAN_POINT('Ctrl Pts',(-33.3478596159751,2.33634667483612,312.37379484819));
#13940=CARTESIAN_POINT('Ctrl Pts',(-33.4260929774439,2.3500176476204,312.379115200164));
#13941=CARTESIAN_POINT('Ctrl Pts',(-33.5049562627513,2.3597448119232,312.384435552138));
#13942=CARTESIAN_POINT('Ctrl Pts',(-33.5840206401277,2.3654972954323,312.389755904112));
#13943=CARTESIAN_POINT('Ctrl Pts',(-33.6646217891527,2.37136158977024,312.395179667589));
#13944=CARTESIAN_POINT('Ctrl Pts',(-33.7454314176383,2.37309504518618,312.400603431066));
#13945=CARTESIAN_POINT('Ctrl Pts',(-33.8259968514571,2.37072062248736,312.406027194543));
#13946=CARTESIAN_POINT('Ctrl Pts',(-33.9065622852758,2.36834619978854,312.41145095802));
#13947=CARTESIAN_POINT('Ctrl Pts',(-33.9868830226482,2.36186400685828,312.416874721497));
#13948=CARTESIAN_POINT('Ctrl Pts',(-34.0665156523982,2.35135215623729,312.422298484974));
#13949=CARTESIAN_POINT('Ctrl Pts',(-34.144799397919,2.34101836415295,312.427630376199));
#13950=CARTESIAN_POINT('Ctrl Pts',(-34.2227148445178,2.32675126035608,312.432962267424));
#13951=CARTESIAN_POINT('Ctrl Pts',(-34.2998358892453,2.30858803897994,312.438294158649));
#13952=CARTESIAN_POINT('Ctrl Pts',(-34.3768453811961,2.29045109004065,312.443618337488));
#13953=CARTESIAN_POINT('Ctrl Pts',(-34.4530623006692,2.26842932159174,312.448942516327));
#13954=CARTESIAN_POINT('Ctrl Pts',(-34.5280672528151,2.24261150170475,312.454266695166));
#13955=CARTESIAN_POINT('Ctrl Pts',(-34.6029848084572,2.21682376499404,312.45958467022));
#13956=CARTESIAN_POINT('Ctrl Pts',(-34.6766927621011,2.18724891850967,312.464902645273));
#13957=CARTESIAN_POINT('Ctrl Pts',(-34.748784970606,2.15402605973946,312.470220620327));
#13958=CARTESIAN_POINT('Ctrl Pts',(-34.8208311760328,2.12082440095462,312.475535201904));
#13959=CARTESIAN_POINT('Ctrl Pts',(-34.8912632580845,2.08397954595495,312.480849783481));
#13960=CARTESIAN_POINT('Ctrl Pts',(-34.9596943622761,2.0436789688604,312.486164365058));
#13961=CARTESIAN_POINT('Ctrl Pts',(-35.0281031208306,2.00339155160127,312.491477211201));
#13962=CARTESIAN_POINT('Ctrl Pts',(-35.0945117953117,1.95965089073064,312.496790057343));
#13963=CARTESIAN_POINT('Ctrl Pts',(-35.1585588163074,1.91269002557991,312.502102903486));
#13964=CARTESIAN_POINT('Ctrl Pts',(-35.2226048781042,1.86572986373761,312.507415670061));
#13965=CARTESIAN_POINT('Ctrl Pts',(-35.2842889794171,1.8155498717802,312.512728436635));
#13966=CARTESIAN_POINT('Ctrl Pts',(-35.3432804155137,1.76242508445002,312.51804120321));
#13967=CARTESIAN_POINT('Ctrl Pts',(-35.40233072613,1.70924727762161,312.523359272022));
#13968=CARTESIAN_POINT('Ctrl Pts',(-35.458682654007,1.65311911893993,312.528677340834));
#13969=CARTESIAN_POINT('Ctrl Pts',(-35.5120408184047,1.59435404271937,312.533995409645));
#13970=CARTESIAN_POINT('Ctrl Pts',(-35.5654245358643,1.53556082408343,312.539316025264));
#13971=CARTESIAN_POINT('Ctrl Pts',(-35.6158113359467,1.47412853518857,312.544636640883));
#13972=CARTESIAN_POINT('Ctrl Pts',(-35.6629464464039,1.4104034024489,312.549957256502));
#13973=CARTESIAN_POINT('Ctrl Pts',(-35.7101675394602,1.34656202403813,312.555287577844));
#13974=CARTESIAN_POINT('Ctrl Pts',(-35.7541248298147,1.28041983552675,312.560617899187));
#13975=CARTESIAN_POINT('Ctrl Pts',(-35.7946072841821,1.2123515564699,312.565948220529));
#13976=CARTESIAN_POINT('Ctrl Pts',(-35.8332431830649,1.14738812508074,312.571035406067));
#13977=CARTESIAN_POINT('Ctrl Pts',(-35.8687142033516,1.08067082032187,312.576122591605));
#13978=CARTESIAN_POINT('Ctrl Pts',(-35.9008777155876,1.01254261087078,312.581209777143));
#13979=CARTESIAN_POINT('Ctrl Pts',(-35.9378642638722,0.934198327761406,
312.587059804719));
#13980=CARTESIAN_POINT('Ctrl Pts',(-35.9706015859964,0.853724764581502,
312.592909832296));
#13981=CARTESIAN_POINT('Ctrl Pts',(-35.9988607118803,0.771585169237672,
312.598759859872));
#13982=CARTESIAN_POINT('Ctrl Pts',(-36.0266549611423,0.690796810933859,
312.604513651597));
#13983=CARTESIAN_POINT('Ctrl Pts',(-36.0501170642415,0.608397144709793,
312.610267443321));
#13984=CARTESIAN_POINT('Ctrl Pts',(-36.0690751867648,0.524851278630692,
312.616021235045));
#13985=CARTESIAN_POINT('Ctrl Pts',(-36.0885089394018,0.439209375365859,
312.621919380548));
#13986=CARTESIAN_POINT('Ctrl Pts',(-36.103209476303,0.352363287906919,312.62781752605));
#13987=CARTESIAN_POINT('Ctrl Pts',(-36.1130445591917,0.26483542197729,312.633715671552));
#13988=CARTESIAN_POINT('Ctrl Pts',(-36.1228796420805,0.177307556047662,
312.639613817055));
#13989=CARTESIAN_POINT('Ctrl Pts',(-36.1278491070246,0.0890982858603586,
312.645511962557));
#13990=CARTESIAN_POINT('Ctrl Pts',(-36.1278769078432,0.000746294306655331,
312.651410108059));
#13991=CARTESIAN_POINT('Ctrl Pts',(-32.6699490794749,2.10841540797709,313.324578124683));
#13992=CARTESIAN_POINT('Ctrl Pts',(-32.6586890743879,2.10261466816627,313.323667641728));
#13993=CARTESIAN_POINT('Ctrl Pts',(-32.64747558103,2.09672374956396,313.322759165335));
#13994=CARTESIAN_POINT('Ctrl Pts',(-32.5641501948446,2.05209406353605,313.315996031982));
#13995=CARTESIAN_POINT('Ctrl Pts',(-32.4940336030402,2.00973173904113,313.310238156099));
#13996=CARTESIAN_POINT('Ctrl Pts',(-32.4000804743237,1.94610740862244,313.302435513491));
#13997=CARTESIAN_POINT('Ctrl Pts',(-32.3742753537587,1.92786991792475,313.300282354887));
#13998=CARTESIAN_POINT('Ctrl Pts',(-32.3308335463775,1.89584731471528,313.296638242202));
#13999=CARTESIAN_POINT('Ctrl Pts',(-32.3130140708035,1.88231867700841,313.295137674329));
#14000=CARTESIAN_POINT('Ctrl Pts',(-32.2767628222872,1.85397910602036,313.292071651396));
#14001=CARTESIAN_POINT('Ctrl Pts',(-32.2583557110656,1.83914059527149,313.290507520255));
#14002=CARTESIAN_POINT('Ctrl Pts',(-32.2115654420805,1.80025310881025,313.286509959624));
#14003=CARTESIAN_POINT('Ctrl Pts',(-32.1835200342395,1.775806644272,313.284092927292));
#14004=CARTESIAN_POINT('Ctrl Pts',(-32.1230854388463,1.72057223386636,313.278826282586));
#14005=CARTESIAN_POINT('Ctrl Pts',(-32.0909675731802,1.68950820967722,313.275988443552));
#14006=CARTESIAN_POINT('Ctrl Pts',(-31.9906577164792,1.5868485972456,313.266959944821));
#14007=CARTESIAN_POINT('Ctrl Pts',(-31.9260557342601,1.51188991338232,313.260890162012));
#14008=CARTESIAN_POINT('Ctrl Pts',(-31.7779476675745,1.31658400306205,313.245867885478));
#14009=CARTESIAN_POINT('Ctrl Pts',(-31.7005563976988,1.19214319748892,313.236966747008));
#14010=CARTESIAN_POINT('Ctrl Pts',(-31.6237939728056,1.03874678103291,313.225836437172));
#14011=CARTESIAN_POINT('Ctrl Pts',(-31.6128271783569,1.01592556875727,313.224176310468));
#14012=CARTESIAN_POINT('Ctrl Pts',(-31.5963208983471,0.980119721610386,
313.221558303073));
#14013=CARTESIAN_POINT('Ctrl Pts',(-31.5905281116862,0.967253066444005,
313.220614897917));
#14014=CARTESIAN_POINT('Ctrl Pts',(-31.5796868526516,0.942587359769649,
313.218799911641));
#14015=CARTESIAN_POINT('Ctrl Pts',(-31.5746187869785,0.930797791944203,
313.217929491182));
#14016=CARTESIAN_POINT('Ctrl Pts',(-31.5622502811555,0.901369685125223,
313.215750462696));
#14017=CARTESIAN_POINT('Ctrl Pts',(-31.5550667574463,0.883683266699383,
313.214435278246));
#14018=CARTESIAN_POINT('Ctrl Pts',(-31.5267975709807,0.811598421728999,
313.209057933878));
#14019=CARTESIAN_POINT('Ctrl Pts',(-31.5075104808776,0.756521156086602,
313.204910681697));
#14020=CARTESIAN_POINT('Ctrl Pts',(-31.4549511171713,0.586582893429965,
313.192106923249));
#14021=CARTESIAN_POINT('Ctrl Pts',(-31.4283136954704,0.46986656769488,313.183311939748));
#14022=CARTESIAN_POINT('Ctrl Pts',(-31.3914779407305,0.224162454293398,
313.165246867116));
#14023=CARTESIAN_POINT('Ctrl Pts',(-31.3827881848785,0.0953216489531737,
313.156026874364));
#14024=CARTESIAN_POINT('Ctrl Pts',(-31.3851067672275,-0.0683014395058179,
313.144730280878));
#14025=CARTESIAN_POINT('Ctrl Pts',(-31.3863598271791,-0.102984465040225,
313.142358043477));
#14026=CARTESIAN_POINT('Ctrl Pts',(-31.3897163209358,-0.160729126179656,
313.138443483193));
#14027=CARTESIAN_POINT('Ctrl Pts',(-31.3913970544757,-0.18380888131378,
313.136888218864));
#14028=CARTESIAN_POINT('Ctrl Pts',(-31.3954169147684,-0.229722647026887,
313.133811526557));
#14029=CARTESIAN_POINT('Ctrl Pts',(-31.3977502638263,-0.252554616421627,
313.132290091853));
#14030=CARTESIAN_POINT('Ctrl Pts',(-31.4043259979175,-0.308812280624378,
313.128560253025));
#14031=CARTESIAN_POINT('Ctrl Pts',(-31.4089499869474,-0.342188886350895,
313.126364032423));
#14032=CARTESIAN_POINT('Ctrl Pts',(-31.4323680839719,-0.488254890763436,
313.116810055559));
#14033=CARTESIAN_POINT('Ctrl Pts',(-31.4585791967774,-0.599605620174556,
313.109686669187));
#14034=CARTESIAN_POINT('Ctrl Pts',(-31.5374058476634,-0.85137789562294,
313.093441540655));
#14035=CARTESIAN_POINT('Ctrl Pts',(-31.5954912572841,-0.989552596102437,
313.08442514723));
#14036=CARTESIAN_POINT('Ctrl Pts',(-31.688513148751,-1.16292721019981,313.071968754634));
#14037=CARTESIAN_POINT('Ctrl Pts',(-31.7120687128626,-1.2038487342366,313.068936080935));
#14038=CARTESIAN_POINT('Ctrl Pts',(-31.7463994266074,-1.25957375859849,
313.064637241868));
#14039=CARTESIAN_POINT('Ctrl Pts',(-31.7561498619814,-1.27499896823074,
313.063428715757));
#14040=CARTESIAN_POINT('Ctrl Pts',(-31.7729835603744,-1.30096165563062,
313.061360132739));
#14041=CARTESIAN_POINT('Ctrl Pts',(-31.7799751384848,-1.3115574500516,313.060505952081));
#14042=CARTESIAN_POINT('Ctrl Pts',(-31.7951161363673,-1.33410780992833,
313.058665781108));
#14043=CARTESIAN_POINT('Ctrl Pts',(-31.8032899797416,-1.34604413039435,
313.057678329311));
#14044=CARTESIAN_POINT('Ctrl Pts',(-31.8270767350198,-1.38010738589654,
313.05482334377));
#14045=CARTESIAN_POINT('Ctrl Pts',(-31.8429595640473,-1.40204191412584,
313.052939436539));
#14046=CARTESIAN_POINT('Ctrl Pts',(-31.9206918008067,-1.50561112080414,
313.043842121119));
#14047=CARTESIAN_POINT('Ctrl Pts',(-31.9874059696796,-1.58344859361498,
313.036397732682));
#14048=CARTESIAN_POINT('Ctrl Pts',(-32.1876948424848,-1.78862993823934,
313.01546527657));
#14049=CARTESIAN_POINT('Ctrl Pts',(-32.3314196618491,-1.90510089161966,
313.002029900501));
#14050=CARTESIAN_POINT('Ctrl Pts',(-32.5186387929183,-2.02366132015657,
312.986688797455));
#14051=CARTESIAN_POINT('Ctrl Pts',(-32.5505365166754,-2.04282502010893,
312.984139608101));
#14052=CARTESIAN_POINT('Ctrl Pts',(-32.6034157070038,-2.07292387120959,
312.98001538703));
#14053=CARTESIAN_POINT('Ctrl Pts',(-32.624132116142,-2.08430908342133,312.978424385611));
#14054=CARTESIAN_POINT('Ctrl Pts',(-32.664996126768,-2.10597789239471,312.975332731625));
#14055=CARTESIAN_POINT('Ctrl Pts',(-32.6851273992073,-2.11628669659473,
312.973831309742));
#14056=CARTESIAN_POINT('Ctrl Pts',(-32.7338717369575,-2.14037392016344,
312.970245593641));
#14057=CARTESIAN_POINT('Ctrl Pts',(-32.7626205123395,-2.15386892794943,
312.968171289395));
#14058=CARTESIAN_POINT('Ctrl Pts',(-32.8738900317796,-2.20339802535053,
312.960285482809));
#14059=CARTESIAN_POINT('Ctrl Pts',(-32.9581707669326,-2.23530163228674,
312.954612079052));
#14060=CARTESIAN_POINT('Ctrl Pts',(-33.2404921192669,-2.32416064156935,
312.936239573021));
#14061=CARTESIAN_POINT('Ctrl Pts',(-33.4440992494008,-2.36013097937297,
312.924032558544));
#14062=CARTESIAN_POINT('Ctrl Pts',(-33.6783814193257,-2.37064854638675,
312.90888509538));
#14063=CARTESIAN_POINT('Ctrl Pts',(-33.7070224163962,-2.37141465570959,
312.907013524308));
#14064=CARTESIAN_POINT('Ctrl Pts',(-33.7504479594286,-2.37178925161856,
312.904136335765));
#14065=CARTESIAN_POINT('Ctrl Pts',(-33.7652276194867,-2.37177858497555,
312.903150162358));
#14066=CARTESIAN_POINT('Ctrl Pts',(-33.7926274681729,-2.37150271026286,
312.901307439557));
#14067=CARTESIAN_POINT('Ctrl Pts',(-33.805247108981,-2.37127488386425,312.900452899957));
#14068=CARTESIAN_POINT('Ctrl Pts',(-33.8355317541939,-2.37048630267468,
312.898388638559));
#14069=CARTESIAN_POINT('Ctrl Pts',(-33.8531931023898,-2.36982880204653,
312.897173867065));
#14070=CARTESIAN_POINT('Ctrl Pts',(-33.9171279475226,-2.36673275251141,
312.892740617524));
#14071=CARTESIAN_POINT('Ctrl Pts',(-33.9633320795099,-2.36313576121074,
312.889469112301));
#14072=CARTESIAN_POINT('Ctrl Pts',(-34.0879321045611,-2.34975366435724,
312.880512707947));
#14073=CARTESIAN_POINT('Ctrl Pts',(-34.1659924381588,-2.33740154073621,
312.874758580285));
#14074=CARTESIAN_POINT('Ctrl Pts',(-34.4173974806705,-2.28463767752996,
312.85599965948));
#14075=CARTESIAN_POINT('Ctrl Pts',(-34.5868761986164,-2.22861509838322,
312.843049912591));
#14076=CARTESIAN_POINT('Ctrl Pts',(-34.7830805105049,-2.13822662378613,
312.82808124603));
#14077=CARTESIAN_POINT('Ctrl Pts',(-34.8172611237326,-2.12147148762995,
312.825471632893));
#14078=CARTESIAN_POINT('Ctrl Pts',(-34.8721417230487,-2.09291087143466,
312.82127606372));
#14079=CARTESIAN_POINT('Ctrl Pts',(-34.8930919882881,-2.08160406088059,
312.819673048284));
#14080=CARTESIAN_POINT('Ctrl Pts',(-34.933526371461,-2.05898910203936,312.816575127921));
#14081=CARTESIAN_POINT('Ctrl Pts',(-34.9530265324101,-2.0477150612715,312.81507921302));
#14082=CARTESIAN_POINT('Ctrl Pts',(-34.999151587765,-2.02016375979472,312.811534373709));
#14083=CARTESIAN_POINT('Ctrl Pts',(-35.025622048016,-2.00363525033919,312.809494840846));
#14084=CARTESIAN_POINT('Ctrl Pts',(-35.1227875307324,-1.94026491931808,
312.801978451707));
#14085=CARTESIAN_POINT('Ctrl Pts',(-35.1912844645948,-1.89016249864544,
312.796622455246));
#14086=CARTESIAN_POINT('Ctrl Pts',(-35.3889896387542,-1.72859284842388,
312.780737267705));
#14087=CARTESIAN_POINT('Ctrl Pts',(-35.5089926288937,-1.60677619342329,
312.770525829199));
#14088=CARTESIAN_POINT('Ctrl Pts',(-35.6511765411855,-1.42737442731966,
312.756153350141));
#14089=CARTESIAN_POINT('Ctrl Pts',(-35.6857530430412,-1.38027267808487,
312.752428972949));
#14090=CARTESIAN_POINT('Ctrl Pts',(-35.7295581294675,-1.31573241103249,
312.747319462395));
#14091=CARTESIAN_POINT('Ctrl Pts',(-35.7403616777977,-1.29938250008593,
312.74602454274));
#14092=CARTESIAN_POINT('Ctrl Pts',(-35.7578834600322,-1.27213718797955,
312.743862490469));
#14093=CARTESIAN_POINT('Ctrl Pts',(-35.7647186044117,-1.26131744956902,
312.743002797603));
#14094=CARTESIAN_POINT('Ctrl Pts',(-35.778783017391,-1.23864983781866,312.741198372929));
#14095=CARTESIAN_POINT('Ctrl Pts',(-35.7859963560826,-1.22679303813002,
312.740252761793));
#14096=CARTESIAN_POINT('Ctrl Pts',(-35.8055102361105,-1.19407413592374,
312.737639971577));
#14097=CARTESIAN_POINT('Ctrl Pts',(-35.8175955757306,-1.17308647941892,
312.735960274613));
#14098=CARTESIAN_POINT('Ctrl Pts',(-35.8886373006526,-1.04522515852139,
312.725721445401));
#14099=CARTESIAN_POINT('Ctrl Pts',(-35.9395879214242,-0.934124607467737,
312.716810603119));
#14100=CARTESIAN_POINT('Ctrl Pts',(-35.9978169286636,-0.77600491013887,
312.70450224756));
#14101=CARTESIAN_POINT('Ctrl Pts',(-36.0125899120188,-0.731937566093798,
312.701108704179));
#14102=CARTESIAN_POINT('Ctrl Pts',(-36.0469688574708,-0.618422027908436,
312.692486011683));
#14103=CARTESIAN_POINT('Ctrl Pts',(-36.0647191292152,-0.548457765586274,
312.68728383032));
#14104=CARTESIAN_POINT('Ctrl Pts',(-36.0929210759187,-0.411332955030435,
312.677344522685));
#14105=CARTESIAN_POINT('Ctrl Pts',(-36.1037319952619,-0.344316284979759,
312.672602533189));
#14106=CARTESIAN_POINT('Ctrl Pts',(-36.115080144577,-0.247787789815633,
312.665937125438));
#14107=CARTESIAN_POINT('Ctrl Pts',(-36.1179645736235,-0.218591257846128,
312.663942234706));
#14108=CARTESIAN_POINT('Ctrl Pts',(-36.1220531485902,-0.16754160781995,
312.660489400263));
#14109=CARTESIAN_POINT('Ctrl Pts',(-36.1234978656349,-0.145711945608564,
312.659024092762));
#14110=CARTESIAN_POINT('Ctrl Pts',(-36.1257396777691,-0.102844534490654,
312.656167350096));
#14111=CARTESIAN_POINT('Ctrl Pts',(-36.1265591135728,-0.0818100484010116,
312.654775347735));
#14112=CARTESIAN_POINT('Ctrl Pts',(-36.1276227136054,-0.0403110232039128,
312.652046917201));
#14113=CARTESIAN_POINT('Ctrl Pts',(-36.1278822476091,-0.0198488686738843,
312.650710146788));
#14114=CARTESIAN_POINT('Ctrl Pts',(-36.1278769456495,0.000614508638078176,
312.64938106027));
#14115=CARTESIAN_POINT('Origin',(-33.7561270252576,0.,307.));
#14116=CARTESIAN_POINT('',(-36.6981270252576,-3.60291088309151E-16,294.));
#14117=CARTESIAN_POINT('Origin',(-33.7561270252576,0.,294.));
#14118=CARTESIAN_POINT('',(-32.4165951196292,2.61935455290104,304.));
#14119=CARTESIAN_POINT('',(-35.045048879311,2.64462557919708,304.));
#14120=CARTESIAN_POINT('Origin',(-33.7561270252576,0.,304.));
#14121=CARTESIAN_POINT('',(-36.6984067016598,0.0019070081496421,304.17782388291));
#14122=CARTESIAN_POINT('Ctrl Pts',(-35.045048879311,2.64462557919709,304.));
#14123=CARTESIAN_POINT('Ctrl Pts',(-35.9252411831751,2.21564269967566,304.052970430723));
#14124=CARTESIAN_POINT('Ctrl Pts',(-36.642667118141,1.20804330944867,304.11224505836));
#14125=CARTESIAN_POINT('Ctrl Pts',(-36.7013903832366,0.117973363423384,
304.171519685997));
#14126=CARTESIAN_POINT('Ctrl Pts',(-36.7004990485223,0.00190836428262659,
304.17782388291));
#14127=CARTESIAN_POINT('',(-36.6981267041397,0.00137457535740912,305.17782388288));
#14128=CARTESIAN_POINT('Ctrl Pts',(-36.6981264073127,0.00190682647975922,
304.17782388291));
#14129=CARTESIAN_POINT('Ctrl Pts',(-36.6981854606991,-0.0892053056498797,
304.182776755507));
#14130=CARTESIAN_POINT('Ctrl Pts',(-36.6940077850111,-0.180500285875559,
304.187729628104));
#14131=CARTESIAN_POINT('Ctrl Pts',(-36.6855688210284,-0.271541461274618,
304.192682500701));
#14132=CARTESIAN_POINT('Ctrl Pts',(-36.6771404656152,-0.362468189374255,
304.197629147072));
#14133=CARTESIAN_POINT('Ctrl Pts',(-36.6644614994644,-0.453141289439652,
304.202575793443));
#14134=CARTESIAN_POINT('Ctrl Pts',(-36.6475593849915,-0.543123290868441,
304.207522439814));
#14135=CARTESIAN_POINT('Ctrl Pts',(-36.6306729670744,-0.633021728343676,
304.212464492363));
#14136=CARTESIAN_POINT('Ctrl Pts',(-36.6095712754905,-0.722229889458937,
304.217406544912));
#14137=CARTESIAN_POINT('Ctrl Pts',(-36.5843335276798,-0.810315975195248,
304.222348597461));
#14138=CARTESIAN_POINT('Ctrl Pts',(-36.55910798703,-0.898359454871054,304.227288259606));
#14139=CARTESIAN_POINT('Ctrl Pts',(-36.5297504869776,-0.985281492292477,
304.23222792175));
#14140=CARTESIAN_POINT('Ctrl Pts',(-36.4963909571031,-1.07066221742735,
304.237167583894));
#14141=CARTESIAN_POINT('Ctrl Pts',(-36.4630374409516,-1.15602755097755,
304.242106355565));
#14142=CARTESIAN_POINT('Ctrl Pts',(-36.4256834960837,-1.23985169331863,
304.247045127237));
#14143=CARTESIAN_POINT('Ctrl Pts',(-36.384507891906,-1.32173296086493,304.251983898908));
#14144=CARTESIAN_POINT('Ctrl Pts',(-36.3433272170591,-1.40362431187755,
304.256923278776));
#14145=CARTESIAN_POINT('Ctrl Pts',(-36.2983241585483,-1.48357190095865,
304.261862658644));
#14146=CARTESIAN_POINT('Ctrl Pts',(-36.2497236632193,-1.56119819598473,
304.266802038513));
#14147=CARTESIAN_POINT('Ctrl Pts',(-36.2010727089338,-1.63890508570063,
304.27174654664));
#14148=CARTESIAN_POINT('Ctrl Pts',(-36.1488171115561,-1.71428548023768,
304.276691054768));
#14149=CARTESIAN_POINT('Ctrl Pts',(-36.0932250918958,-1.78699094203527,
304.281635562896));
#14150=CARTESIAN_POINT('Ctrl Pts',(-36.037600203778,-1.8597393905131,304.286582994435));
#14151=CARTESIAN_POINT('Ctrl Pts',(-35.9786352690852,-1.92980940885522,
304.291530425975));
#14152=CARTESIAN_POINT('Ctrl Pts',(-35.9166371470862,-1.99688758158193,
304.296477857514));
#14153=CARTESIAN_POINT('Ctrl Pts',(-35.854540124742,-2.06407275842786,304.301433181271));
#14154=CARTESIAN_POINT('Ctrl Pts',(-35.7894005919193,-2.1282562461531,304.306388505029));
#14155=CARTESIAN_POINT('Ctrl Pts',(-35.7215600172065,-2.18916357409825,
304.311343828786));
#14156=CARTESIAN_POINT('Ctrl Pts',(-35.6919943405294,-2.21570766475376,
304.31350341397));
#14157=CARTESIAN_POINT('Ctrl Pts',(-35.6619160432118,-2.2416300539507,304.315662999154));
#14158=CARTESIAN_POINT('Ctrl Pts',(-35.6313550759192,-2.2669106197669,304.317822584338));
#14159=CARTESIAN_POINT('Ctrl Pts',(-35.5598720168902,-2.32604265447061,
304.322873921677));
#14160=CARTESIAN_POINT('Ctrl Pts',(-35.4854586911232,-2.38189825448609,
304.327925259016));
#14161=CARTESIAN_POINT('Ctrl Pts',(-35.4084480715605,-2.43417319842788,
304.332976596355));
#14162=CARTESIAN_POINT('Ctrl Pts',(-35.3315455516945,-2.48637476410539,
304.338020843139));
#14163=CARTESIAN_POINT('Ctrl Pts',(-35.2520533470419,-2.53500541361462,
304.343065089923));
#14164=CARTESIAN_POINT('Ctrl Pts',(-35.170338012154,-2.5798006288358,304.348109336707));
#14165=CARTESIAN_POINT('Ctrl Pts',(-35.0887120906379,-2.62454682888449,
304.353148064049));
#14166=CARTESIAN_POINT('Ctrl Pts',(-35.004868261466,-2.66546572358029,304.35818679139));
#14167=CARTESIAN_POINT('Ctrl Pts',(-34.919201690894,-2.70233627110963,304.363225518731));
#14168=CARTESIAN_POINT('Ctrl Pts',(-34.8335998302158,-2.73917896776087,
304.368260439973));
#14169=CARTESIAN_POINT('Ctrl Pts',(-34.7461783720883,-2.77197922066161,
304.373295361214));
#14170=CARTESIAN_POINT('Ctrl Pts',(-34.6573557382733,-2.80056258755918,
304.378330282456));
#14171=CARTESIAN_POINT('Ctrl Pts',(-34.5685672970876,-2.82913495117493,
304.383363265484));
#14172=CARTESIAN_POINT('Ctrl Pts',(-34.4783791744485,-2.85349351759961,
304.388396248512));
#14173=CARTESIAN_POINT('Ctrl Pts',(-34.3872273957038,-2.8735128888562,304.393429231541));
#14174=CARTESIAN_POINT('Ctrl Pts',(-34.296085166436,-2.89353016279196,304.398461687291));
#14175=CARTESIAN_POINT('Ctrl Pts',(-34.2039799159809,-2.90920905013263,
304.403494143041));
#14176=CARTESIAN_POINT('Ctrl Pts',(-34.1113592482792,-2.92047497296709,
304.408526598791));
#14177=CARTESIAN_POINT('Ctrl Pts',(-34.0187223329283,-2.93174287208575,
304.413559937341));
#14178=CARTESIAN_POINT('Ctrl Pts',(-33.9255702621046,-2.9385962161771,304.418593275892));
#14179=CARTESIAN_POINT('Ctrl Pts',(-33.832356019879,-2.94101226457473,304.423626614443));
#14180=CARTESIAN_POINT('Ctrl Pts',(-33.7390420287663,-2.94343089839423,
304.428665339186));
#14181=CARTESIAN_POINT('Ctrl Pts',(-33.6456661785347,-2.94140274649516,
304.43370406393));
#14182=CARTESIAN_POINT('Ctrl Pts',(-33.5526813899142,-2.93495721833551,
304.438742788674));
#14183=CARTESIAN_POINT('Ctrl Pts',(-33.4596410362822,-2.92850783851526,
304.443784524414));
#14184=CARTESIAN_POINT('Ctrl Pts',(-33.3669926507445,-2.91763587886526,
304.448826260153));
#14185=CARTESIAN_POINT('Ctrl Pts',(-33.2751817983903,-2.90242238289909,
304.453867995893));
#14186=CARTESIAN_POINT('Ctrl Pts',(-33.1832243190797,-2.88718459014716,
304.45891778356));
#14187=CARTESIAN_POINT('Ctrl Pts',(-33.0921074774406,-2.86759151198321,
304.463967571227));
#14188=CARTESIAN_POINT('Ctrl Pts',(-33.002264267968,-2.84377477012013,304.469017358895));
#14189=CARTESIAN_POINT('Ctrl Pts',(-32.956501504991,-2.83164341462688,304.471589531433));
#14190=CARTESIAN_POINT('Ctrl Pts',(-32.9110689104682,-2.81841702045556,
304.47416170397));
#14191=CARTESIAN_POINT('Ctrl Pts',(-32.8660217096371,-2.80411778053349,
304.476733876508));
#14192=CARTESIAN_POINT('Ctrl Pts',(-32.7774092731068,-2.77598971782041,
304.481793602119));
#14193=CARTESIAN_POINT('Ctrl Pts',(-32.6899775587321,-2.74360836087013,
304.48685332773));
#14194=CARTESIAN_POINT('Ctrl Pts',(-32.6041635777236,-2.70709146789421,
304.491913053341));
#14195=CARTESIAN_POINT('Ctrl Pts',(-32.5184654773731,-2.67062388624883,
304.496965946448));
#14196=CARTESIAN_POINT('Ctrl Pts',(-32.4343811730132,-2.63003203869568,
304.502018839556));
#14197=CARTESIAN_POINT('Ctrl Pts',(-32.3523321918021,-2.58548333306629,
304.507071732663));
#14198=CARTESIAN_POINT('Ctrl Pts',(-32.270368876532,-2.54098113998017,304.512119350131));
#14199=CARTESIAN_POINT('Ctrl Pts',(-32.1904370472337,-2.49253051133187,
304.517166967599));
#14200=CARTESIAN_POINT('Ctrl Pts',(-32.1129369193408,-2.4403463434146,304.522214585067));
#14201=CARTESIAN_POINT('Ctrl Pts',(-32.0354902433746,-2.38819816697764,
304.527258721187));
#14202=CARTESIAN_POINT('Ctrl Pts',(-31.960472301415,-2.33232181619026,304.532302857307));
#14203=CARTESIAN_POINT('Ctrl Pts',(-31.8882565289755,-2.27297686066506,
304.537346993428));
#14204=CARTESIAN_POINT('Ctrl Pts',(-31.8160656728214,-2.2136523806648,304.542389389192));
#14205=CARTESIAN_POINT('Ctrl Pts',(-31.7466754070349,-2.15086195445824,
304.547431784957));
#14206=CARTESIAN_POINT('Ctrl Pts',(-31.6804272817949,-2.08490637079679,
304.552474180722));
#14207=CARTESIAN_POINT('Ctrl Pts',(-31.6141836406136,-2.01895525139302,
304.557516235187));
#14208=CARTESIAN_POINT('Ctrl Pts',(-31.5510820306443,-1.94983971306171,
304.562558289653));
#14209=CARTESIAN_POINT('Ctrl Pts',(-31.4914273986124,-1.87789765457896,
304.567600344119));
#14210=CARTESIAN_POINT('Ctrl Pts',(-31.4317602600743,-1.8059405135491,304.572643455645));
#14211=CARTESIAN_POINT('Ctrl Pts',(-31.3755418171684,-1.7311560163198,304.57768656717));
#14212=CARTESIAN_POINT('Ctrl Pts',(-31.3230362369419,-1.65391451284924,
304.582729678695));
#14213=CARTESIAN_POINT('Ctrl Pts',(-31.2704724489103,-1.57658737927302,
304.587778381025));
#14214=CARTESIAN_POINT('Ctrl Pts',(-31.221629989032,-1.49679816901213,304.592827083355));
#14215=CARTESIAN_POINT('Ctrl Pts',(-31.1767290702231,-1.41494529560819,
304.597875785685));
#14216=CARTESIAN_POINT('Ctrl Pts',(-31.1318002081743,-1.33304148261251,
304.60292762998));
#14217=CARTESIAN_POINT('Ctrl Pts',(-31.0908179649267,-1.24907184707223,
304.607979474275));
#14218=CARTESIAN_POINT('Ctrl Pts',(-31.0539551055439,-1.16345645226235,
304.613031318569));
#14219=CARTESIAN_POINT('Ctrl Pts',(-31.0170327261524,-1.07770281996536,
304.618091319741));
#14220=CARTESIAN_POINT('Ctrl Pts',(-30.9842431645956,-0.990298537332545,
304.623151320913));
#14221=CARTESIAN_POINT('Ctrl Pts',(-30.9557098242559,-0.901680375927937,
304.628211322085));
#14222=CARTESIAN_POINT('Ctrl Pts',(-30.9417366736823,-0.858282901320502,
304.630689270949));
#14223=CARTESIAN_POINT('Ctrl Pts',(-30.9287834717208,-0.814594498065602,
304.633167219813));
#14224=CARTESIAN_POINT('Ctrl Pts',(-30.9168602232918,-0.770667261050437,
304.635645168677));
#14225=CARTESIAN_POINT('Ctrl Pts',(-30.8925677055117,-0.681169571508969,
304.640693760694));
#14226=CARTESIAN_POINT('Ctrl Pts',(-30.8724667729455,-0.590359276240205,
304.645742352711));
#14227=CARTESIAN_POINT('Ctrl Pts',(-30.8566965402011,-0.498665080314254,
304.650790944728));
#14228=CARTESIAN_POINT('Ctrl Pts',(-30.8409482211076,-0.40709829877985,
304.655832521434));
#14229=CARTESIAN_POINT('Ctrl Pts',(-30.8295187190975,-0.314650491811056,
304.66087409814));
#14230=CARTESIAN_POINT('Ctrl Pts',(-30.8224971057688,-0.221764504553785,
304.665915674846));
#14231=CARTESIAN_POINT('Ctrl Pts',(-30.8154830707788,-0.128978767971246,
304.670951810242));
#14232=CARTESIAN_POINT('Ctrl Pts',(-30.8128675022509,-0.0357562323716657,
304.675987945638));
#14233=CARTESIAN_POINT('Ctrl Pts',(-30.8146880502506,0.0574522089200695,
304.681024081034));
#14234=CARTESIAN_POINT('Ctrl Pts',(-30.8165072681548,0.150592551962246,
304.686056537021));
#14235=CARTESIAN_POINT('Ctrl Pts',(-30.8227561520802,0.243718377546381,
304.691088993008));
#14236=CARTESIAN_POINT('Ctrl Pts',(-30.8334203043104,0.336376906653812,
304.696121448994));
#14237=CARTESIAN_POINT('Ctrl Pts',(-30.8440805176586,0.429001211661709,
304.701152046207));
#14238=CARTESIAN_POINT('Ctrl Pts',(-30.8591527088614,0.521158121429664,
304.70618264342));
#14239=CARTESIAN_POINT('Ctrl Pts',(-30.8785705473647,0.612399148053428,
304.711213240632));
#14240=CARTESIAN_POINT('Ctrl Pts',(-30.8979866680719,0.703632103053712,
304.716243392814));
#14241=CARTESIAN_POINT('Ctrl Pts',(-30.921747578977,0.793948900766828,304.721273544995));
#14242=CARTESIAN_POINT('Ctrl Pts',(-30.9497358979465,0.882911570062178,
304.726303697177));
#14243=CARTESIAN_POINT('Ctrl Pts',(-30.9777296025736,0.971891358016018,
304.731334817287));
#14244=CARTESIAN_POINT('Ctrl Pts',(-31.0099521968002,1.05951607572889,304.736365937396));
#14245=CARTESIAN_POINT('Ctrl Pts',(-31.0462368920462,1.14536433763394,304.741397057506));
#14246=CARTESIAN_POINT('Ctrl Pts',(-31.0825614605805,1.23130693828065,304.746433706318));
#14247=CARTESIAN_POINT('Ctrl Pts',(-31.122956866943,1.31546877587347,304.751470355131));
#14248=CARTESIAN_POINT('Ctrl Pts',(-31.1672088839136,1.39745012698849,304.756507003943));
#14249=CARTESIAN_POINT('Ctrl Pts',(-31.2114880394619,1.47948175507192,304.761546741598));
#14250=CARTESIAN_POINT('Ctrl Pts',(-31.2596282843582,1.55932985381511,304.766586479252));
#14251=CARTESIAN_POINT('Ctrl Pts',(-31.3113714564842,1.63662280594869,304.771626216907));
#14252=CARTESIAN_POINT('Ctrl Pts',(-31.3631987410459,1.71404140361594,304.776674147036));
#14253=CARTESIAN_POINT('Ctrl Pts',(-31.4186403806381,1.78889620548035,304.781722077164));
#14254=CARTESIAN_POINT('Ctrl Pts',(-31.4773973968817,1.86084800044545,304.786770007293));
#14255=CARTESIAN_POINT('Ctrl Pts',(-31.5076083788235,1.89784331636418,304.789365491811));
#14256=CARTESIAN_POINT('Ctrl Pts',(-31.5386952293429,1.9340717539159,304.791960976329));
#14257=CARTESIAN_POINT('Ctrl Pts',(-31.5706136604705,1.96949113537912,304.794556460846));
#14258=CARTESIAN_POINT('Ctrl Pts',(-31.6327474971313,2.03844007756441,304.799608946366));
#14259=CARTESIAN_POINT('Ctrl Pts',(-31.6982589083538,2.10456961592866,304.804661431885));
#14260=CARTESIAN_POINT('Ctrl Pts',(-31.766861969177,2.16753051573831,304.809713917405));
#14261=CARTESIAN_POINT('Ctrl Pts',(-31.8353703396491,2.23040451286983,304.814759429159));
#14262=CARTESIAN_POINT('Ctrl Pts',(-31.9069615556201,2.29011826452337,304.819804940914));
#14263=CARTESIAN_POINT('Ctrl Pts',(-31.981310754738,2.34635700734113,304.824850452668));
#14264=CARTESIAN_POINT('Ctrl Pts',(-32.0555802999834,2.4025354988892,304.829890558923));
#14265=CARTESIAN_POINT('Ctrl Pts',(-32.1326016029631,2.45524611498477,304.834930665178));
#14266=CARTESIAN_POINT('Ctrl Pts',(-32.2120152378283,2.50421300769759,304.839970771433));
#14267=CARTESIAN_POINT('Ctrl Pts',(-32.2913714757742,2.553144509148,304.845007234906));
#14268=CARTESIAN_POINT('Ctrl Pts',(-32.373116231767,2.59833743295884,304.850043698379));
#14269=CARTESIAN_POINT('Ctrl Pts',(-32.4568603529284,2.63955869686101,304.855080161852));
#14270=CARTESIAN_POINT('Ctrl Pts',(-32.5405739207141,2.68076492151328,304.860114787811));
#14271=CARTESIAN_POINT('Ctrl Pts',(-32.6262850063833,2.71800216893644,304.865149413771));
#14272=CARTESIAN_POINT('Ctrl Pts',(-32.7135799813971,2.75108336139379,304.87018403973));
#14273=CARTESIAN_POINT('Ctrl Pts',(-32.8008675225753,2.78416173673429,304.875218236952));
#14274=CARTESIAN_POINT('Ctrl Pts',(-32.8897382694725,2.81308460353882,304.880252434175));
#14275=CARTESIAN_POINT('Ctrl Pts',(-32.979759821264,2.83771350995184,304.885286631397));
#14276=CARTESIAN_POINT('Ctrl Pts',(-33.0697988843359,2.86234720725854,304.890321807888));
#14277=CARTESIAN_POINT('Ctrl Pts',(-33.1609887683415,2.88268516846175,304.895356984378));
#14278=CARTESIAN_POINT('Ctrl Pts',(-33.2528842838104,2.89863946415913,304.900392160869));
#14279=CARTESIAN_POINT('Ctrl Pts',(-33.3448805646758,2.91461125408268,304.905432858538));
#14280=CARTESIAN_POINT('Ctrl Pts',(-33.437583583138,2.92618970747071,304.910473556207));
#14281=CARTESIAN_POINT('Ctrl Pts',(-33.5305406876089,2.93333850829839,304.915514253876));
#14282=CARTESIAN_POINT('Ctrl Pts',(-33.6235547875403,2.94049169232194,304.920558042184));
#14283=CARTESIAN_POINT('Ctrl Pts',(-33.716822839926,2.94320980382093,304.925601830493));
#14284=CARTESIAN_POINT('Ctrl Pts',(-33.8098920317969,2.94150868162442,304.930645618801));
#14285=CARTESIAN_POINT('Ctrl Pts',(-33.9031117125039,2.93980480878729,304.935697562696));
#14286=CARTESIAN_POINT('Ctrl Pts',(-33.9961314480596,2.93366746590286,304.940749506591));
#14287=CARTESIAN_POINT('Ctrl Pts',(-34.0885035655184,2.92316435314271,304.945801450486));
#14288=CARTESIAN_POINT('Ctrl Pts',(-34.1352283255008,2.91785154407991,304.948356884663));
#14289=CARTESIAN_POINT('Ctrl Pts',(-34.1817875400494,2.91142249892789,304.950912318839));
#14290=CARTESIAN_POINT('Ctrl Pts',(-34.2281245246065,2.90389090025923,304.953467753016));
#14291=CARTESIAN_POINT('Ctrl Pts',(-34.3197490134596,2.88899828510833,304.958520743677));
#14292=CARTESIAN_POINT('Ctrl Pts',(-34.4108318991177,2.86973832589534,304.963573734339));
#14293=CARTESIAN_POINT('Ctrl Pts',(-34.5009246691104,2.8461624109863,304.968626725));
#14294=CARTESIAN_POINT('Ctrl Pts',(-34.5908934455138,2.82261894332369,304.973672761291));
#14295=CARTESIAN_POINT('Ctrl Pts',(-34.6798743881723,2.7947714350649,304.978718797583));
#14296=CARTESIAN_POINT('Ctrl Pts',(-34.7674268960541,2.76272267361873,304.983764833874));
#14297=CARTESIAN_POINT('Ctrl Pts',(-34.8548859364688,2.73070812611603,304.988805483224));
#14298=CARTESIAN_POINT('Ctrl Pts',(-34.9409191583632,2.69450139213777,304.993846132574));
#14299=CARTESIAN_POINT('Ctrl Pts',(-35.025099974914,2.6542553857985,304.998886781924));
#14300=CARTESIAN_POINT('Ctrl Pts',(-35.1092203804635,2.61403826135463,305.003923813933));
#14301=CARTESIAN_POINT('Ctrl Pts',(-35.1914906234124,2.56978781717587,305.008960845943));
#14302=CARTESIAN_POINT('Ctrl Pts',(-35.2715039831891,2.52170511269069,305.013997877952));
#14303=CARTESIAN_POINT('Ctrl Pts',(-35.3514884017069,2.47363979997609,305.019033088041));
#14304=CARTESIAN_POINT('Ctrl Pts',(-35.429217178504,2.42174520923741,305.024068298129));
#14305=CARTESIAN_POINT('Ctrl Pts',(-35.5043090261056,2.36626788253385,305.029103508217));
#14306=CARTESIAN_POINT('Ctrl Pts',(-35.5793947021467,2.31079511533554,305.034138304477));
#14307=CARTESIAN_POINT('Ctrl Pts',(-35.6518435228012,2.25174046167026,305.039173100737));
#14308=CARTESIAN_POINT('Ctrl Pts',(-35.7213049238018,2.18939257034307,305.044207896998));
#14309=CARTESIAN_POINT('Ctrl Pts',(-35.7907800314854,2.12703237602788,305.049243686764));
#14310=CARTESIAN_POINT('Ctrl Pts',(-35.8572662185125,2.06137795033843,305.054279476531));
#14311=CARTESIAN_POINT('Ctrl Pts',(-35.9204484764443,1.99275604526325,305.059315266298));
#14312=CARTESIAN_POINT('Ctrl Pts',(-35.9837002323473,1.92405865882124,305.064356595233));
#14313=CARTESIAN_POINT('Ctrl Pts',(-36.0436405035994,1.85238760466307,305.069397924169));
#14314=CARTESIAN_POINT('Ctrl Pts',(-36.0999936365512,1.77810385199042,305.074439253104));
#14315=CARTESIAN_POINT('Ctrl Pts',(-36.1563814422621,1.70377439426943,305.07948368385));
#14316=CARTESIAN_POINT('Ctrl Pts',(-36.2091774646966,1.62682940365229,305.084528114597));
#14317=CARTESIAN_POINT('Ctrl Pts',(-36.2581498129686,1.54765822124098,305.089572545344));
#14318=CARTESIAN_POINT('Ctrl Pts',(-36.3072014459971,1.46835886307041,305.094625142872));
#14319=CARTESIAN_POINT('Ctrl Pts',(-36.3524168313347,1.3868265057755,305.099677740399));
#14320=CARTESIAN_POINT('Ctrl Pts',(-36.3936104632933,1.30347424757353,305.104730337927));
#14321=CARTESIAN_POINT('Ctrl Pts',(-36.4143970013056,1.26141423001381,305.107279907013));
#14322=CARTESIAN_POINT('Ctrl Pts',(-36.4341602616885,1.21889112438577,305.109829476099));
#14323=CARTESIAN_POINT('Ctrl Pts',(-36.452881187343,1.1759596035897,305.112379045185));
#14324=CARTESIAN_POINT('Ctrl Pts',(-36.4937574003875,1.08222075633557,305.117945902885));
#14325=CARTESIAN_POINT('Ctrl Pts',(-36.5297871600594,0.986245715449588,
305.123512760585));
#14326=CARTESIAN_POINT('Ctrl Pts',(-36.5607450233516,0.888527931337765,
305.129079618284));
#14327=CARTESIAN_POINT('Ctrl Pts',(-36.5916177368753,0.791078920513456,
305.134631164312));
#14328=CARTESIAN_POINT('Ctrl Pts',(-36.617446262904,0.69189698993402,305.14018271034));
#14329=CARTESIAN_POINT('Ctrl Pts',(-36.6380530834695,0.591494881633886,
305.145734256368));
#14330=CARTESIAN_POINT('Ctrl Pts',(-36.6585600993455,0.491579049283951,
305.15125891468));
#14331=CARTESIAN_POINT('Ctrl Pts',(-36.6738957476405,0.390455097248779,
305.156783572993));
#14332=CARTESIAN_POINT('Ctrl Pts',(-36.6839327803678,0.288647640461142,
305.162308231305));
#14333=CARTESIAN_POINT('Ctrl Pts',(-36.6933289030985,0.193341050867358,
305.167480115163));
#14334=CARTESIAN_POINT('Ctrl Pts',(-36.6980818219432,0.0974358112860457,
305.172651999022));
#14335=CARTESIAN_POINT('Ctrl Pts',(-36.6981267041397,0.00137457535742581,
305.17782388288));
#14336=CARTESIAN_POINT('',(-36.6981259159627,-0.00255481704953209,306.177823882956));
#14337=CARTESIAN_POINT('Ctrl Pts',(-36.69812670414,0.00137457480061522,
305.17782388291));
#14338=CARTESIAN_POINT('Ctrl Pts',(-36.6981711145098,-0.0936768503563982,
305.182941399114));
#14339=CARTESIAN_POINT('Ctrl Pts',(-36.6936047326977,-0.188714855235633,
305.188058915319));
#14340=CARTESIAN_POINT('Ctrl Pts',(-36.6844578460534,-0.2832712551197,305.193176431524));
#14341=CARTESIAN_POINT('Ctrl Pts',(-36.6753071449356,-0.377867087315354,
305.198296081856));
#14342=CARTESIAN_POINT('Ctrl Pts',(-36.6615721793269,-0.471980493434233,
305.203415732189));
#14343=CARTESIAN_POINT('Ctrl Pts',(-36.6433349537333,-0.565149871934047,
305.208535382522));
#14344=CARTESIAN_POINT('Ctrl Pts',(-36.6247061380591,-0.660319785232445,
305.213764962092));
#14345=CARTESIAN_POINT('Ctrl Pts',(-36.6013795804879,-0.754504207632462,
305.218994541661));
#14346=CARTESIAN_POINT('Ctrl Pts',(-36.5734968599925,-0.847225598247542,
305.22422412123));
#14347=CARTESIAN_POINT('Ctrl Pts',(-36.54613897342,-0.938201702523416,305.229355264897));
#14348=CARTESIAN_POINT('Ctrl Pts',(-36.5143951653034,-1.02776899639892,
305.234486408564));
#14349=CARTESIAN_POINT('Ctrl Pts',(-36.4784481532836,-1.11549615683031,
305.23961755223));
#14350=CARTESIAN_POINT('Ctrl Pts',(-36.4414667295986,-1.20574775512201,
305.244896349751));
#14351=CARTESIAN_POINT('Ctrl Pts',(-36.4000367303914,-1.29405126427797,
305.250175147272));
#14352=CARTESIAN_POINT('Ctrl Pts',(-36.3544073594601,-1.37996496509757,
305.255453944793));
#14353=CARTESIAN_POINT('Ctrl Pts',(-36.3087779885287,-1.46587866591718,
305.260732742313));
#14354=CARTESIAN_POINT('Ctrl Pts',(-36.2589495538321,-1.54940218336193,
305.266011539834));
#14355=CARTESIAN_POINT('Ctrl Pts',(-36.2052180200171,-1.63012800092138,
305.271290337355));
#14356=CARTESIAN_POINT('Ctrl Pts',(-36.1537916608698,-1.70739054288728,
305.276342665437));
#14357=CARTESIAN_POINT('Ctrl Pts',(-36.0986132638484,-1.78235581499684,
305.281394993518));
#14358=CARTESIAN_POINT('Ctrl Pts',(-36.0399148375032,-1.85463668373043,
305.2864473216));
#14359=CARTESIAN_POINT('Ctrl Pts',(-35.9812973679311,-1.92681786280866,
305.291492681519));
#14360=CARTESIAN_POINT('Ctrl Pts',(-35.9191697938031,-1.9963216536412,305.296538041438));
#14361=CARTESIAN_POINT('Ctrl Pts',(-35.853807665721,-2.0627893568237,305.301583401357));
#14362=CARTESIAN_POINT('Ctrl Pts',(-35.7885154902605,-2.12918592416307,
305.306623361572));
#14363=CARTESIAN_POINT('Ctrl Pts',(-35.7199959513547,-2.19255254731278,
305.311663321787));
#14364=CARTESIAN_POINT('Ctrl Pts',(-35.6485644612311,-2.25256399485696,
305.316703282002));
#14365=CARTESIAN_POINT('Ctrl Pts',(-35.5771844683521,-2.3125321782303,305.321739608749));
#14366=CARTESIAN_POINT('Ctrl Pts',(-35.5028970361107,-2.36914970887272,
305.326775935495));
#14367=CARTESIAN_POINT('Ctrl Pts',(-35.4260532144577,-2.4221293364772,305.331812262242));
#14368=CARTESIAN_POINT('Ctrl Pts',(-35.3492373402543,-2.47508969583817,
305.336846757319));
#14369=CARTESIAN_POINT('Ctrl Pts',(-35.2698672890388,-2.52441452868439,
305.341881252396));
#14370=CARTESIAN_POINT('Ctrl Pts',(-35.1883250236095,-2.56985853570132,
305.346915747473));
#14371=CARTESIAN_POINT('Ctrl Pts',(-35.1067896045841,-2.61529872717515,
305.351949819846));
#14372=CARTESIAN_POINT('Ctrl Pts',(-35.0230827221049,-2.65685852456116,
305.35698389222));
#14373=CARTESIAN_POINT('Ctrl Pts',(-34.9376119904645,-2.6943380034788,305.362017964594));
#14374=CARTESIAN_POINT('Ctrl Pts',(-34.8521245266221,-2.73182481957722,
305.367053022464));
#14375=CARTESIAN_POINT('Ctrl Pts',(-34.7648729348238,-2.76522955276159,
305.372088080334));
#14376=CARTESIAN_POINT('Ctrl Pts',(-34.6762848366658,-2.79440040117814,
305.377123138204));
#14377=CARTESIAN_POINT('Ctrl Pts',(-34.5875994170297,-2.82360329622559,
305.382163727509));
#14378=CARTESIAN_POINT('Ctrl Pts',(-34.4975749828143,-2.84856288283961,
305.387204316814));
#14379=CARTESIAN_POINT('Ctrl Pts',(-34.4066540525099,-2.86917733624367,
305.392244906119));
#14380=CARTESIAN_POINT('Ctrl Pts',(-34.315677271657,-2.88980445261239,305.397288591737));
#14381=CARTESIAN_POINT('Ctrl Pts',(-34.2238033354969,-2.90608104464846,
305.402332277355));
#14382=CARTESIAN_POINT('Ctrl Pts',(-34.1314825136292,-2.91795686351757,
305.407375962973));
#14383=CARTESIAN_POINT('Ctrl Pts',(-34.0390122288789,-2.92985190875497,
305.412427814071));
#14384=CARTESIAN_POINT('Ctrl Pts',(-33.9460940563293,-2.93733192175819,
305.417479665169));
#14385=CARTESIAN_POINT('Ctrl Pts',(-33.8531807296274,-2.94039871079895,
305.422531516266));
#14386=CARTESIAN_POINT('Ctrl Pts',(-33.8061579832348,-2.94195079001537,
305.425088220685));
#14387=CARTESIAN_POINT('Ctrl Pts',(-33.7591364404184,-2.94237334174126,
305.427644925105));
#14388=CARTESIAN_POINT('Ctrl Pts',(-33.7121742597644,-2.94167165985694,
305.430201629524));
#14389=CARTESIAN_POINT('Ctrl Pts',(-33.6193715853836,-2.94028505568902,
305.435253971736));
#14390=CARTESIAN_POINT('Ctrl Pts',(-33.5264680640071,-2.93450010510437,
305.440306313949));
#14391=CARTESIAN_POINT('Ctrl Pts',(-33.4339147939597,-2.9243021865057,305.445358656161));
#14392=CARTESIAN_POINT('Ctrl Pts',(-33.3414891459972,-2.91411832985895,
305.450404031678));
#14393=CARTESIAN_POINT('Ctrl Pts',(-33.2494132273939,-2.89953364522624,
305.455449407195));
#14394=CARTESIAN_POINT('Ctrl Pts',(-33.1581378141286,-2.88058551398379,
305.460494782712));
#14395=CARTESIAN_POINT('Ctrl Pts',(-33.0669600603847,-2.86165765616839,
305.465534759963));
#14396=CARTESIAN_POINT('Ctrl Pts',(-32.9765815421969,-2.8383757211902,305.470574737214));
#14397=CARTESIAN_POINT('Ctrl Pts',(-32.8874464882813,-2.81082872560364,
305.475614714464));
#14398=CARTESIAN_POINT('Ctrl Pts',(-32.7983756576732,-2.78330157809133,
305.480651060327));
#14399=CARTESIAN_POINT('Ctrl Pts',(-32.7105469337537,-2.7515156088772,305.485687406189));
#14400=CARTESIAN_POINT('Ctrl Pts',(-32.6243919166768,-2.71561036306861,
305.490723752052));
#14401=CARTESIAN_POINT('Ctrl Pts',(-32.5382682113436,-2.679718166481,305.49575826753));
#14402=CARTESIAN_POINT('Ctrl Pts',(-32.4538174140773,-2.63970983814811,
305.500792783009));
#14403=CARTESIAN_POINT('Ctrl Pts',(-32.3714526001545,-2.59577362966524,
305.505827298487));
#14404=CARTESIAN_POINT('Ctrl Pts',(-32.2890946809843,-2.55184109907919,
305.510861392526));
#14405=CARTESIAN_POINT('Ctrl Pts',(-32.2088227898532,-2.50398155132848,
305.515895486566));
#14406=CARTESIAN_POINT('Ctrl Pts',(-32.1310257494574,-2.45242937582157,
305.520929580605));
#14407=CARTESIAN_POINT('Ctrl Pts',(-32.0532134599363,-2.4008670954883,305.525964661386));
#14408=CARTESIAN_POINT('Ctrl Pts',(-31.9778773546524,-2.34561099561574,
305.530999742166));
#14409=CARTESIAN_POINT('Ctrl Pts',(-31.9053766372575,-2.28693834663676,
305.536034822947));
#14410=CARTESIAN_POINT('Ctrl Pts',(-31.8327962467274,-2.22820122058678,
305.541075436923));
#14411=CARTESIAN_POINT('Ctrl Pts',(-31.7630578096342,-2.16604033081065,
305.546116050899));
#14412=CARTESIAN_POINT('Ctrl Pts',(-31.6964865840428,-2.10077253716643,
305.551156664876));
#14413=CARTESIAN_POINT('Ctrl Pts',(-31.6298744518257,-2.03546463782815,
305.556200376204));
#14414=CARTESIAN_POINT('Ctrl Pts',(-31.5664337074163,-1.96704635943276,
305.561244087532));
#14415=CARTESIAN_POINT('Ctrl Pts',(-31.5064504491303,-1.89586900993298,
305.56628779886));
#14416=CARTESIAN_POINT('Ctrl Pts',(-31.446370065043,-1.82457640898968,305.571339677042));
#14417=CARTESIAN_POINT('Ctrl Pts',(-31.3897586130749,-1.75051617056496,
305.576391555224));
#14418=CARTESIAN_POINT('Ctrl Pts',(-31.3368597640667,-1.6740698668006,305.581443433406));
#14419=CARTESIAN_POINT('Ctrl Pts',(-31.3100903733426,-1.63538431856568,
305.583999929502));
#14420=CARTESIAN_POINT('Ctrl Pts',(-31.2842710071267,-1.59608815225124,
305.586556425598));
#14421=CARTESIAN_POINT('Ctrl Pts',(-31.2594287056429,-1.55623311262589,
305.589112921693));
#14422=CARTESIAN_POINT('Ctrl Pts',(-31.2103345269535,-1.47747026376844,
305.594165153919));
#14423=CARTESIAN_POINT('Ctrl Pts',(-31.1648829387026,-1.39624058813763,
305.599217386146));
#14424=CARTESIAN_POINT('Ctrl Pts',(-31.1233305500467,-1.3129153514667,305.604269618372));
#14425=CARTESIAN_POINT('Ctrl Pts',(-31.0818354756799,-1.22970504745927,
305.609314881923));
#14426=CARTESIAN_POINT('Ctrl Pts',(-31.0442291101545,-1.14440532024443,
305.614360145474));
#14427=CARTESIAN_POINT('Ctrl Pts',(-31.0107241737315,-1.05741533128288,
305.619405409025));
#14428=CARTESIAN_POINT('Ctrl Pts',(-30.9772550985143,-0.970518449971734,
305.624445272499));
#14429=CARTESIAN_POINT('Ctrl Pts',(-30.947878885703,-0.881935315182517,
305.629485135974));
#14430=CARTESIAN_POINT('Ctrl Pts',(-30.9227613040443,-0.792087551886581,
305.634524999448));
#14431=CARTESIAN_POINT('Ctrl Pts',(-30.8976618315003,-0.702304566460958,
305.639561229313));
#14432=CARTESIAN_POINT('Ctrl Pts',(-30.8768150066068,-0.611259191416344,
305.644597459178));
#14433=CARTESIAN_POINT('Ctrl Pts',(-30.8603372828654,-0.519389803381136,
305.649633689044));
#14434=CARTESIAN_POINT('Ctrl Pts',(-30.84386555221,-0.427553829011225,305.65466808719));
#14435=CARTESIAN_POINT('Ctrl Pts',(-30.831759844188,-0.334894873883701,
305.659702485337));
#14436=CARTESIAN_POINT('Ctrl Pts',(-30.8240856351023,-0.241862122739805,
305.664736883483));
#14437=CARTESIAN_POINT('Ctrl Pts',(-30.8164120702546,-0.148837181552168,
305.669770859));
#14438=CARTESIAN_POINT('Ctrl Pts',(-30.8131693010271,-0.0554389495150576,
305.674804834516));
#14439=CARTESIAN_POINT('Ctrl Pts',(-30.8143708835112,0.0378787869061924,
305.679838810033));
#14440=CARTESIAN_POINT('Ctrl Pts',(-30.8155727012748,0.131214795689443,
305.684873771242));
#14441=CARTESIAN_POINT('Ctrl Pts',(-30.8212205929581,0.224469833356506,
305.689908732451));
#14442=CARTESIAN_POINT('Ctrl Pts',(-30.8312760256051,0.317191787144155,
305.69494369366));
#14443=CARTESIAN_POINT('Ctrl Pts',(-30.8413425069902,0.410015622235569,
305.699984187199));
#14444=CARTESIAN_POINT('Ctrl Pts',(-30.8558261484302,0.502304761874496,
305.705024680738));
#14445=CARTESIAN_POINT('Ctrl Pts',(-30.8746367516526,0.593614187094206,
305.710065174277));
#14446=CARTESIAN_POINT('Ctrl Pts',(-30.8934589113658,0.684979709214852,
305.715108764496));
#14447=CARTESIAN_POINT('Ctrl Pts',(-30.9166132148726,0.77536388860677,305.720152354715));
#14448=CARTESIAN_POINT('Ctrl Pts',(-30.9439592965877,0.864335968144081,
305.725195944934));
#14449=CARTESIAN_POINT('Ctrl Pts',(-30.9713496592894,0.953452118466536,
305.730247702142));
#14450=CARTESIAN_POINT('Ctrl Pts',(-31.0029452005464,1.04115118660185,305.73529945935));
#14451=CARTESIAN_POINT('Ctrl Pts',(-31.0385571348216,1.12702169038389,305.740351216558));
#14452=CARTESIAN_POINT('Ctrl Pts',(-31.056587182879,1.1704972651151,305.742908882326));
#14453=CARTESIAN_POINT('Ctrl Pts',(-31.0756460196631,1.21350449811005,305.745466548094));
#14454=CARTESIAN_POINT('Ctrl Pts',(-31.0957047499967,1.2559925625956,305.748024213862));
#14455=CARTESIAN_POINT('Ctrl Pts',(-31.1353277645684,1.33992136418171,305.753076499142));
#14456=CARTESIAN_POINT('Ctrl Pts',(-31.1789973687618,1.42212398259354,305.758128784422));
#14457=CARTESIAN_POINT('Ctrl Pts',(-31.2265404258993,1.5021836227129,305.763181069703));
#14458=CARTESIAN_POINT('Ctrl Pts',(-31.274017912798,1.58213284650578,305.768226386993));
#14459=CARTESIAN_POINT('Ctrl Pts',(-31.3253580121973,1.6599445863842,305.773271704283));
#14460=CARTESIAN_POINT('Ctrl Pts',(-31.3803403677703,1.73522383515941,305.778317021573));
#14461=CARTESIAN_POINT('Ctrl Pts',(-31.4352638815194,1.81042252048378,305.783356939391));
#14462=CARTESIAN_POINT('Ctrl Pts',(-31.4938216431132,1.8830937449263,305.788396857209));
#14463=CARTESIAN_POINT('Ctrl Pts',(-31.5557489845037,1.95286980563684,305.793436775028));
#14464=CARTESIAN_POINT('Ctrl Pts',(-31.6176316866468,2.02259556948712,305.798473059909));
#14465=CARTESIAN_POINT('Ctrl Pts',(-31.6828788467583,2.08942998635647,305.80350934479));
#14466=CARTESIAN_POINT('Ctrl Pts',(-31.7511850065142,2.15303773805229,305.808545629671));
#14467=CARTESIAN_POINT('Ctrl Pts',(-31.8194663283909,2.21662236033099,305.813580083229));
#14468=CARTESIAN_POINT('Ctrl Pts',(-31.8908041153576,2.27698234586884,305.818614536788));
#14469=CARTESIAN_POINT('Ctrl Pts',(-31.9648562151284,2.33381937706824,305.823648990346));
#14470=CARTESIAN_POINT('Ctrl Pts',(-32.0389021032213,2.39065164063333,305.828683021601));
#14471=CARTESIAN_POINT('Ctrl Pts',(-32.1156614989019,2.44396126706701,305.833717052857));
#14472=CARTESIAN_POINT('Ctrl Pts',(-32.1947602624996,2.49349109325755,305.838751084113));
#14473=CARTESIAN_POINT('Ctrl Pts',(-32.2738745181639,2.54303062022381,305.84378610132));
#14474=CARTESIAN_POINT('Ctrl Pts',(-32.3553286749949,2.58878864126048,305.848821118527));
#14475=CARTESIAN_POINT('Ctrl Pts',(-32.4387217898061,2.63055268823968,305.853856135734));
#14476=CARTESIAN_POINT('Ctrl Pts',(-32.5222065353734,2.67236262475317,305.858896685321));
#14477=CARTESIAN_POINT('Ctrl Pts',(-32.6076340937918,2.71016962799671,305.863937234909));
#14478=CARTESIAN_POINT('Ctrl Pts',(-32.6945815041307,2.74380850399137,305.868977784496));
#14479=CARTESIAN_POINT('Ctrl Pts',(-32.7815823328632,2.77746804690081,305.874021430876));
#14480=CARTESIAN_POINT('Ctrl Pts',(-32.8701044512753,2.8069542242249,305.879065077255));
#14481=CARTESIAN_POINT('Ctrl Pts',(-32.9597097176111,2.83215173888708,305.884108723635));
#14482=CARTESIAN_POINT('Ctrl Pts',(-33.0494600717647,2.85739005307551,305.889160536629));
#14483=CARTESIAN_POINT('Ctrl Pts',(-33.1402966427661,2.8783257418025,305.894212349623));
#14484=CARTESIAN_POINT('Ctrl Pts',(-33.2317712685927,2.89489465101105,305.899264162617));
#14485=CARTESIAN_POINT('Ctrl Pts',(-33.2780736732506,2.90328146136399,305.901821277089));
#14486=CARTESIAN_POINT('Ctrl Pts',(-33.3245394738246,2.91055026116043,305.90437839156));
#14487=CARTESIAN_POINT('Ctrl Pts',(-33.3711103324178,2.91669781537868,305.906935506032));
#14488=CARTESIAN_POINT('Ctrl Pts',(-33.463123866918,2.92884399883414,305.911987788678));
#14489=CARTESIAN_POINT('Ctrl Pts',(-33.5558778885821,2.93665356560635,305.917040071324));
#14490=CARTESIAN_POINT('Ctrl Pts',(-33.6489282527769,2.94004633010751,305.922092353969));
#14491=CARTESIAN_POINT('Ctrl Pts',(-33.7418502857503,2.94343441544792,305.927137668715));
#14492=CARTESIAN_POINT('Ctrl Pts',(-33.8350674090016,2.94241778699734,305.932182983462));
#14493=CARTESIAN_POINT('Ctrl Pts',(-33.9281282201202,2.93696775415833,305.937228298208));
#14494=CARTESIAN_POINT('Ctrl Pts',(-34.021089439732,2.93152355381719,305.942268213576));
#14495=CARTESIAN_POINT('Ctrl Pts',(-34.113894238596,2.9216554053822,305.947308128944));
#14496=CARTESIAN_POINT('Ctrl Pts',(-34.2060901687657,2.90738665634351,305.952348044312));
#14497=CARTESIAN_POINT('Ctrl Pts',(-34.2982196438287,2.89312819226249,305.957384326893));
#14498=CARTESIAN_POINT('Ctrl Pts',(-34.3897406847555,2.87447550005484,305.962420609475));
#14499=CARTESIAN_POINT('Ctrl Pts',(-34.4802059759686,2.85150375646556,305.967456892057));
#14500=CARTESIAN_POINT('Ctrl Pts',(-34.5706383733567,2.82854036556609,305.97249134341));
#14501=CARTESIAN_POINT('Ctrl Pts',(-34.6600153534899,2.80126115235585,305.977525794764));
#14502=CARTESIAN_POINT('Ctrl Pts',(-34.7479008320584,2.76979217923366,305.982560246117));
#14503=CARTESIAN_POINT('Ctrl Pts',(-34.8357789402739,2.73832584519863,305.987594275266));
#14504=CARTESIAN_POINT('Ctrl Pts',(-34.9221653774275,2.702670599785,305.992628304414));
#14505=CARTESIAN_POINT('Ctrl Pts',(-35.0066413314548,2.66300168418949,305.997662333563));
#14506=CARTESIAN_POINT('Ctrl Pts',(-35.0911338324131,2.62332499834962,306.002697348764));
#14507=CARTESIAN_POINT('Ctrl Pts',(-35.1737147050978,2.57963327011389,306.007732363965));
#14508=CARTESIAN_POINT('Ctrl Pts',(-35.2539881935179,2.53214847918087,306.012767379166));
#14509=CARTESIAN_POINT('Ctrl Pts',(-35.3343498876031,2.48461151127571,306.017807926914));
#14510=CARTESIAN_POINT('Ctrl Pts',(-35.412398753533,2.43327338764073,306.022848474663));
#14511=CARTESIAN_POINT('Ctrl Pts',(-35.4877668514603,2.37840020019946,306.027889022411));
#14512=CARTESIAN_POINT('Ctrl Pts',(-35.5631812551253,2.32349329897871,306.032932667044));
#14513=CARTESIAN_POINT('Ctrl Pts',(-35.6359112657968,2.2650472881556,306.037976311676));
#14514=CARTESIAN_POINT('Ctrl Pts',(-35.7056226673916,2.20336804490324,306.043019956309));
#14515=CARTESIAN_POINT('Ctrl Pts',(-35.7754469471574,2.14158892931992,306.048071767717));
#14516=CARTESIAN_POINT('Ctrl Pts',(-35.8422425420291,2.07656643913191,306.053123579126));
#14517=CARTESIAN_POINT('Ctrl Pts',(-35.9057128021194,2.00864257345936,306.058175390534));
#14518=CARTESIAN_POINT('Ctrl Pts',(-35.9378403038885,1.97426073680938,306.060732526423));
#14519=CARTESIAN_POINT('Ctrl Pts',(-35.9691164376634,1.93913602754469,306.063289662312));
#14520=CARTESIAN_POINT('Ctrl Pts',(-35.999506887958,1.90331573619042,306.065846798201));
#14521=CARTESIAN_POINT('Ctrl Pts',(-36.0591447921124,1.83302236831168,306.070864895122));
#14522=CARTESIAN_POINT('Ctrl Pts',(-36.1155911972667,1.7597869486787,306.075882992043));
#14523=CARTESIAN_POINT('Ctrl Pts',(-36.1685392712908,1.68393323952848,306.080901088964));
#14524=CARTESIAN_POINT('Ctrl Pts',(-36.2214185594307,1.6081780734235,306.085912666777));
#14525=CARTESIAN_POINT('Ctrl Pts',(-36.2708082843961,1.52981173657589,306.09092424459));
#14526=CARTESIAN_POINT('Ctrl Pts',(-36.316440565194,1.44919238792459,306.095935822403));
#14527=CARTESIAN_POINT('Ctrl Pts',(-36.3620267530452,1.36865447248823,306.100942338045));
#14528=CARTESIAN_POINT('Ctrl Pts',(-36.403862813887,1.28586845454363,306.105948853687));
#14529=CARTESIAN_POINT('Ctrl Pts',(-36.4417237757902,1.20122191685325,306.110955369329));
#14530=CARTESIAN_POINT('Ctrl Pts',(-36.479557433727,1.11663642320685,306.115958274452));
#14531=CARTESIAN_POINT('Ctrl Pts',(-36.5134215051908,1.0301934856244,306.120961179575));
#14532=CARTESIAN_POINT('Ctrl Pts',(-36.5431372321584,0.942304678238938,
306.125964084698));
#14533=CARTESIAN_POINT('Ctrl Pts',(-36.5728451955578,0.854438832793723,
306.130965682756));
#14534=CARTESIAN_POINT('Ctrl Pts',(-36.5984068163879,0.765128291939525,
306.135967280813));
#14535=CARTESIAN_POINT('Ctrl Pts',(-36.6196920864541,0.67480303814878,306.140968878871));
#14536=CARTESIAN_POINT('Ctrl Pts',(-36.6409740365617,0.584491872790789,
306.145969696807));
#14537=CARTESIAN_POINT('Ctrl Pts',(-36.6579808638972,0.493166748923216,
306.150970514743));
#14538=CARTESIAN_POINT('Ctrl Pts',(-36.6706332603493,0.40126974170949,306.155971332679));
#14539=CARTESIAN_POINT('Ctrl Pts',(-36.6832914889933,0.30933037406389,306.160974455769));
#14540=CARTESIAN_POINT('Ctrl Pts',(-36.6915912226164,0.216819044003163,
306.16597757886));
#14541=CARTESIAN_POINT('Ctrl Pts',(-36.6955049036665,0.124184088836673,
306.170980701951));
#14542=CARTESIAN_POINT('Ctrl Pts',(-36.6972892576362,0.0819492853693997,
306.17326176227));
#14543=CARTESIAN_POINT('Ctrl Pts',(-36.6981626001127,0.0396888201570203,
306.17554282259));
#14544=CARTESIAN_POINT('Ctrl Pts',(-36.6981259159634,-0.00255481619919655,
306.17782388291));
#14545=CARTESIAN_POINT('',(-36.6981270248952,-4.61744834887231E-5,307.177823883003));
#14546=CARTESIAN_POINT('Ctrl Pts',(-36.6981259159627,-0.00255481704952955,
306.177823882956));
#14547=CARTESIAN_POINT('Ctrl Pts',(-36.6980278861538,-0.115441017225031,
306.183919481112));
#14548=CARTESIAN_POINT('Ctrl Pts',(-36.6914288167197,-0.228042423400951,
306.190015079268));
#14549=CARTESIAN_POINT('Ctrl Pts',(-36.678449336265,-0.33970032468089,306.196110677424));
#14550=CARTESIAN_POINT('Ctrl Pts',(-36.66528380746,-0.452958734425924,306.202293650108));
#14551=CARTESIAN_POINT('Ctrl Pts',(-36.6455537081551,-0.565246414805456,
306.208476622792));
#14552=CARTESIAN_POINT('Ctrl Pts',(-36.6194337914689,-0.675898189499465,
306.214659595477));
#14553=CARTESIAN_POINT('Ctrl Pts',(-36.6052134555697,-0.736139783027078,
306.218025760441));
#14554=CARTESIAN_POINT('Ctrl Pts',(-36.5891000237347,-0.795896879811981,
306.221391925406));
#14555=CARTESIAN_POINT('Ctrl Pts',(-36.5711275860838,-0.855064817746686,
306.22475809037));
#14556=CARTESIAN_POINT('Ctrl Pts',(-36.544152748426,-0.943869995505168,
306.229810368487));
#14557=CARTESIAN_POINT('Ctrl Pts',(-36.5129230489886,-1.03155685598148,
306.234862646604));
#14558=CARTESIAN_POINT('Ctrl Pts',(-36.4775490641029,-1.1176878305175,306.23991492472));
#14559=CARTESIAN_POINT('Ctrl Pts',(-36.442223866422,-1.20370001466287,306.24496023482));
#14560=CARTESIAN_POINT('Ctrl Pts',(-36.4027659084823,-1.28816016956632,
306.25000554492));
#14561=CARTESIAN_POINT('Ctrl Pts',(-36.3593356563898,-1.3706454037419,306.25505085502));
#14562=CARTESIAN_POINT('Ctrl Pts',(-36.3159518833297,-1.45304236226443,
306.260090765631));
#14563=CARTESIAN_POINT('Ctrl Pts',(-36.2686044717746,-1.53346821009158,
306.265130676243));
#14564=CARTESIAN_POINT('Ctrl Pts',(-36.2175017042479,-1.61152061408643,
306.270170586854));
#14565=CARTESIAN_POINT('Ctrl Pts',(-36.1664357732496,-1.68951675538271,
306.275206864535));
#14566=CARTESIAN_POINT('Ctrl Pts',(-36.1116201094323,-1.76514248279957,
306.280243142216));
#14567=CARTESIAN_POINT('Ctrl Pts',(-36.0533080678788,-1.83802156065203,
306.285279419897));
#14568=CARTESIAN_POINT('Ctrl Pts',(-35.995017230037,-1.91087413785538,306.290313866262));
#14569=CARTESIAN_POINT('Ctrl Pts',(-35.933232817441,-1.98098170308195,306.295348312627));
#14570=CARTESIAN_POINT('Ctrl Pts',(-35.8682498774875,-2.0479992815156,306.300382758992));
#14571=CARTESIAN_POINT('Ctrl Pts',(-35.8032723882692,-2.11501123854948,
306.30541678307));
#14572=CARTESIAN_POINT('Ctrl Pts',(-35.7350972145074,-2.17893340530029,
306.310450807148));
#14573=CARTESIAN_POINT('Ctrl Pts',(-35.6640570446037,-2.23945686300899,
306.315484831226));
#14574=CARTESIAN_POINT('Ctrl Pts',(-35.5930029605927,-2.29999217499513,
306.320519841281));
#14575=CARTESIAN_POINT('Ctrl Pts',(-35.5190831043916,-2.35712716808914,
306.325554851336));
#14576=CARTESIAN_POINT('Ctrl Pts',(-35.4426631925446,-2.41059323744859,
306.33058986139));
#14577=CARTESIAN_POINT('Ctrl Pts',(-35.3661593105919,-2.46411805525971,
306.335630403908));
#14578=CARTESIAN_POINT('Ctrl Pts',(-35.2871502541142,-2.5139656470969,306.340670946426));
#14579=CARTESIAN_POINT('Ctrl Pts',(-35.2060304087611,-2.55991097081618,
306.345711488944));
#14580=CARTESIAN_POINT('Ctrl Pts',(-35.1248607246741,-2.6058845226066,306.35075512829));
#14581=CARTESIAN_POINT('Ctrl Pts',(-35.0415780662161,-2.64795083319799,
306.355798767636));
#14582=CARTESIAN_POINT('Ctrl Pts',(-34.9565991061602,-2.68593201384052,
306.360842406982));
#14583=CARTESIAN_POINT('Ctrl Pts',(-34.8714825468343,-2.72397469420872,
306.365894213069));
#14584=CARTESIAN_POINT('Ctrl Pts',(-34.7846646157423,-2.75791887761006,
306.370946019155));
#14585=CARTESIAN_POINT('Ctrl Pts',(-34.6965793487808,-2.78763581322592,
306.375997825242));
#14586=CARTESIAN_POINT('Ctrl Pts',(-34.6519912575088,-2.8026782997083,306.378555011008));
#14587=CARTESIAN_POINT('Ctrl Pts',(-34.6070786392107,-2.81663844150935,
306.381112196774));
#14588=CARTESIAN_POINT('Ctrl Pts',(-34.561898743212,-2.82950453941054,306.38366938254));
#14589=CARTESIAN_POINT('Ctrl Pts',(-34.4726360188751,-2.85492431793941,
306.388721659954));
#14590=CARTESIAN_POINT('Ctrl Pts',(-34.3820090100032,-2.87616160923423,
306.393773937368));
#14591=CARTESIAN_POINT('Ctrl Pts',(-34.2904454424642,-2.89307238572315,
306.398826214782));
#14592=CARTESIAN_POINT('Ctrl Pts',(-34.1990081578266,-2.90995983915926,
306.403871524181));
#14593=CARTESIAN_POINT('Ctrl Pts',(-34.1066373143415,-2.92253255510016,
306.408916833581));
#14594=CARTESIAN_POINT('Ctrl Pts',(-34.0137753194199,-2.93069639446246,
306.41396214298));
#14595=CARTESIAN_POINT('Ctrl Pts',(-33.9210127053026,-2.9388514968929,306.419002052895));
#14596=CARTESIAN_POINT('Ctrl Pts',(-33.8277604246888,-2.94260706252909,
306.42404196281));
#14597=CARTESIAN_POINT('Ctrl Pts',(-33.734469499653,-2.94192028300984,306.429081872725));
#14598=CARTESIAN_POINT('Ctrl Pts',(-33.6412458215886,-2.94123399854241,
306.434118149718));
#14599=CARTESIAN_POINT('Ctrl Pts',(-33.5479839974368,-2.93611173695885,
306.43915442671));
#14600=CARTESIAN_POINT('Ctrl Pts',(-33.4551375214818,-2.9265627139388,306.444190703703));
#14601=CARTESIAN_POINT('Ctrl Pts',(-33.3623248067228,-2.91701716317156,
306.449225149385));
#14602=CARTESIAN_POINT('Ctrl Pts',(-33.2699275816022,-2.9030480941656,306.454259595067));
#14603=CARTESIAN_POINT('Ctrl Pts',(-33.1783956413144,-2.88471670151629,
306.45929404075));
#14604=CARTESIAN_POINT('Ctrl Pts',(-33.0868713785632,-2.86638684647166,
306.464328064151));
#14605=CARTESIAN_POINT('Ctrl Pts',(-32.9962126919121,-2.84369548270597,
306.469362087553));
#14606=CARTESIAN_POINT('Ctrl Pts',(-32.9068594522753,-2.81675497505209,
306.474396110955));
#14607=CARTESIAN_POINT('Ctrl Pts',(-32.8174887115554,-2.7898091907226,306.47943112034));
#14608=CARTESIAN_POINT('Ctrl Pts',(-32.7294243508627,-2.75861273823514,
306.484466129726));
#14609=CARTESIAN_POINT('Ctrl Pts',(-32.6430902392105,-2.72332758090282,
306.489501139112));
#14610=CARTESIAN_POINT('Ctrl Pts',(-32.556661263468,-2.68800365217077,306.494541680976));
#14611=CARTESIAN_POINT('Ctrl Pts',(-32.4719667436607,-2.64858221901239,
306.49958222284));
#14612=CARTESIAN_POINT('Ctrl Pts',(-32.3894094550258,-2.6052729383348,306.504622764703));
#14613=CARTESIAN_POINT('Ctrl Pts',(-32.3068014443821,-2.5619370490591,306.509666403404));
#14614=CARTESIAN_POINT('Ctrl Pts',(-32.2263336618595,-2.51470878166137,
306.514710042104));
#14615=CARTESIAN_POINT('Ctrl Pts',(-32.1483813140059,-2.46384206635727,
306.519753680804));
#14616=CARTESIAN_POINT('Ctrl Pts',(-32.0703027441829,-2.41289298667088,
306.524805486263));
#14617=CARTESIAN_POINT('Ctrl Pts',(-31.994748099982,-2.35829395741093,306.529857291721));
#14618=CARTESIAN_POINT('Ctrl Pts',(-31.9220606841871,-2.30034011758097,
306.53490909718));
#14619=CARTESIAN_POINT('Ctrl Pts',(-31.8852667663045,-2.27100424423385,
306.53746628969));
#14620=CARTESIAN_POINT('Ctrl Pts',(-31.8492069570012,-2.24080936811905,
306.540023482199));
#14621=CARTESIAN_POINT('Ctrl Pts',(-31.8139220971151,-2.20979727963877,
306.542580674709));
#14622=CARTESIAN_POINT('Ctrl Pts',(-31.744209368765,-2.14852631790696,306.547632951162));
#14623=CARTESIAN_POINT('Ctrl Pts',(-31.6772737338398,-2.08384328835132,
306.552685227615));
#14624=CARTESIAN_POINT('Ctrl Pts',(-31.6134679200877,-2.01602975152468,
306.557737504069));
#14625=CARTESIAN_POINT('Ctrl Pts',(-31.5497501064817,-1.94830974224348,
306.562782812488));
#14626=CARTESIAN_POINT('Ctrl Pts',(-31.4891538381885,-1.87746812596406,
306.567828120907));
#14627=CARTESIAN_POINT('Ctrl Pts',(-31.4319978559518,-1.80382582429177,
306.572873429327));
#14628=CARTESIAN_POINT('Ctrl Pts',(-31.3749030421993,-1.7302623348067,306.577913338244));
#14629=CARTESIAN_POINT('Ctrl Pts',(-31.3212414672872,-1.65390446658554,
306.582953247161));
#14630=CARTESIAN_POINT('Ctrl Pts',(-31.2712933867857,-1.57510818330629,
306.587993156078));
#14631=CARTESIAN_POINT('Ctrl Pts',(-31.2213813106296,-1.49636869917867,
306.59302943205));
#14632=CARTESIAN_POINT('Ctrl Pts',(-31.175177645499,-1.41519466780222,306.598065708022));
#14633=CARTESIAN_POINT('Ctrl Pts',(-31.1329202522621,-1.33197230681066,
306.603101983994));
#14634=CARTESIAN_POINT('Ctrl Pts',(-31.0906782249401,-1.24878020768858,
306.608136428642));
#14635=CARTESIAN_POINT('Ctrl Pts',(-31.0523798197239,-1.1635416543478,306.61317087329));
#14636=CARTESIAN_POINT('Ctrl Pts',(-31.0182171983976,-1.0766679060804,306.618205317938));
#14637=CARTESIAN_POINT('Ctrl Pts',(-30.984057442656,-0.989801444843948,
306.623239340293));
#14638=CARTESIAN_POINT('Ctrl Pts',(-30.9540329434734,-0.901300474894601,
306.628273362648));
#14639=CARTESIAN_POINT('Ctrl Pts',(-30.9282874718564,-0.811595626047812,
306.633307385003));
#14640=CARTESIAN_POINT('Ctrl Pts',(-30.9025369576843,-0.721873207445191,
306.638342393331));
#14641=CARTESIAN_POINT('Ctrl Pts',(-30.8810672577357,-0.630946868751912,
306.643377401659));
#14642=CARTESIAN_POINT('Ctrl Pts',(-30.8639717819456,-0.539260649948624,
306.648412409987));
#14643=CARTESIAN_POINT('Ctrl Pts',(-30.8468575216451,-0.447473686319338,
306.653452950783));
#14644=CARTESIAN_POINT('Ctrl Pts',(-30.8341271612002,-0.354925613313889,
306.658493491578));
#14645=CARTESIAN_POINT('Ctrl Pts',(-30.825822593093,-0.26206856895959,306.663534032374));
#14646=CARTESIAN_POINT('Ctrl Pts',(-30.8175129227902,-0.169154474702264,
306.668577669998));
#14647=CARTESIAN_POINT('Ctrl Pts',(-30.813634476547,-0.0759314747314025,
306.673621307622));
#14648=CARTESIAN_POINT('Ctrl Pts',(-30.8141769978822,0.0171474903620899,
306.678664945247));
#14649=CARTESIAN_POINT('Ctrl Pts',(-30.8147203976786,0.11037717074817,306.683716749628));
#14650=CARTESIAN_POINT('Ctrl Pts',(-30.8196990324575,0.203461907586567,
306.68876855401));
#14651=CARTESIAN_POINT('Ctrl Pts',(-30.8290507251081,0.295953261687169,
306.693820358392));
#14652=CARTESIAN_POINT('Ctrl Pts',(-30.833784513888,0.342772008906082,306.696377561221));
#14653=CARTESIAN_POINT('Ctrl Pts',(-30.8396380121032,0.389438859133182,
306.698934764049));
#14654=CARTESIAN_POINT('Ctrl Pts',(-30.8465982077714,0.435896845844663,
306.701491966878));
#14655=CARTESIAN_POINT('Ctrl Pts',(-30.8603494975764,0.527684098601365,
306.706544243979));
#14656=CARTESIAN_POINT('Ctrl Pts',(-30.8784731646952,0.618984748438965,
306.711596521079));
#14657=CARTESIAN_POINT('Ctrl Pts',(-30.9009235509167,0.709349786855151,
306.71664879818));
#14658=CARTESIAN_POINT('Ctrl Pts',(-30.9233429739038,0.799590195172318,
306.721694107256));
#14659=CARTESIAN_POINT('Ctrl Pts',(-30.950077151935,0.888897128811458,306.726739416332));
#14660=CARTESIAN_POINT('Ctrl Pts',(-30.9810289311959,0.97682883266996,306.731784725408));
#14661=CARTESIAN_POINT('Ctrl Pts',(-31.011947585836,1.06466643194327,306.73682463499));
#14662=CARTESIAN_POINT('Ctrl Pts',(-31.0470747233719,1.15113131000311,306.741864544572));
#14663=CARTESIAN_POINT('Ctrl Pts',(-31.0862628889441,1.23579508561368,306.746904454154));
#14664=CARTESIAN_POINT('Ctrl Pts',(-31.1254228063775,1.32039783274682,306.7519407308));
#14665=CARTESIAN_POINT('Ctrl Pts',(-31.1686377473062,1.40320165596974,306.756977007447));
#14666=CARTESIAN_POINT('Ctrl Pts',(-31.2157118635612,1.48379742762378,306.762013284094));
#14667=CARTESIAN_POINT('Ctrl Pts',(-31.2627688624683,1.56436389260216,306.767047729422));
#14668=CARTESIAN_POINT('Ctrl Pts',(-31.3136820250735,1.64272351783683,306.77208217475));
#14669=CARTESIAN_POINT('Ctrl Pts',(-31.36820970196,1.71849202997719,306.777116620079));
#14670=CARTESIAN_POINT('Ctrl Pts',(-31.4227328050804,1.79425418667629,306.782150643119));
#14671=CARTESIAN_POINT('Ctrl Pts',(-31.4808695600314,1.86742530192697,306.78718466616));
#14672=CARTESIAN_POINT('Ctrl Pts',(-31.5423358257536,1.937651290867,306.7922186892));
#14673=CARTESIAN_POINT('Ctrl Pts',(-31.6038141304191,2.00789103445263,306.797253698217));
#14674=CARTESIAN_POINT('Ctrl Pts',(-31.6686229481257,2.0751841720915,306.802288707235));
#14675=CARTESIAN_POINT('Ctrl Pts',(-31.7364395896121,2.13921169179105,306.807323716252));
#14676=CARTESIAN_POINT('Ctrl Pts',(-31.8043307480469,2.20330956495084,306.812364257739));
#14677=CARTESIAN_POINT('Ctrl Pts',(-31.8752360038975,2.26413435212009,306.817404799226));
#14678=CARTESIAN_POINT('Ctrl Pts',(-31.9487979590096,2.32140596326777,306.822445340713));
#14679=CARTESIAN_POINT('Ctrl Pts',(-32.0224051094515,2.37871276120936,306.827488979031));
#14680=CARTESIAN_POINT('Ctrl Pts',(-32.0986718457472,2.43246178144004,306.832532617349));
#14681=CARTESIAN_POINT('Ctrl Pts',(-32.1772118517246,2.48241633792307,306.837576255666));
#14682=CARTESIAN_POINT('Ctrl Pts',(-32.255879031155,2.53245178176226,306.842628060738));
#14683=CARTESIAN_POINT('Ctrl Pts',(-32.3368264434786,2.5786802759391,306.84767986581));
#14684=CARTESIAN_POINT('Ctrl Pts',(-32.4196434369083,2.62091121903678,306.852731670882));
#14685=CARTESIAN_POINT('Ctrl Pts',(-32.4615649453431,2.64228829110816,306.855288866937));
#14686=CARTESIAN_POINT('Ctrl Pts',(-32.5039651833339,2.6626418269809,306.857846062993));
#14687=CARTESIAN_POINT('Ctrl Pts',(-32.5467892156698,2.68195191274964,306.860403259048));
#14688=CARTESIAN_POINT('Ctrl Pts',(-32.6313970706085,2.72010303599651,306.865455536032));
#14689=CARTESIAN_POINT('Ctrl Pts',(-32.7179639015626,2.75431501252238,306.870507813015));
#14690=CARTESIAN_POINT('Ctrl Pts',(-32.8060875247434,2.78438304610961,306.875560089999));
#14691=CARTESIAN_POINT('Ctrl Pts',(-32.8940896091405,2.81440961031446,306.880605398957));
#14692=CARTESIAN_POINT('Ctrl Pts',(-32.983643802389,2.84030344631984,306.885650707916));
#14693=CARTESIAN_POINT('Ctrl Pts',(-33.0743261287194,2.86190697568591,306.890696016875));
#14694=CARTESIAN_POINT('Ctrl Pts',(-33.1649114067385,2.88348738493448,306.895735926339));
#14695=CARTESIAN_POINT('Ctrl Pts',(-33.256621988251,2.90078651142073,306.900775835803));
#14696=CARTESIAN_POINT('Ctrl Pts',(-33.3490178975942,2.91369630506907,306.905815745267));
#14697=CARTESIAN_POINT('Ctrl Pts',(-33.4413472048798,2.92659679290694,306.910852021796));
#14698=CARTESIAN_POINT('Ctrl Pts',(-33.5343604193706,2.9351141754558,306.915888298325));
#14699=CARTESIAN_POINT('Ctrl Pts',(-33.6276075414581,2.93919151167186,306.920924574855));
#14700=CARTESIAN_POINT('Ctrl Pts',(-33.7208207565177,2.94326736526465,306.925959020065));
#14701=CARTESIAN_POINT('Ctrl Pts',(-33.8142672668187,2.94290636054046,306.930993465276));
#14702=CARTESIAN_POINT('Ctrl Pts',(-33.9074931608555,2.9381035197886,306.936027910487));
#14703=CARTESIAN_POINT('Ctrl Pts',(-34.0007112351353,2.93330108189743,306.94106193341));
#14704=CARTESIAN_POINT('Ctrl Pts',(-34.0937082862849,2.92405757179393,306.946095956333));
#14705=CARTESIAN_POINT('Ctrl Pts',(-34.1860327674912,2.91042008184293,306.951129979256));
#14706=CARTESIAN_POINT('Ctrl Pts',(-34.278375331619,2.89677992081641,306.956164988157));
#14707=CARTESIAN_POINT('Ctrl Pts',(-34.3700446247773,2.87874413603468,306.961199997057));
#14708=CARTESIAN_POINT('Ctrl Pts',(-34.4605977065936,2.85641122024437,306.966235005958));
#14709=CARTESIAN_POINT('Ctrl Pts',(-34.5512502881931,2.83405376503216,306.971275547329));
#14710=CARTESIAN_POINT('Ctrl Pts',(-34.6407837782241,2.80738986030109,306.9763160887));
#14711=CARTESIAN_POINT('Ctrl Pts',(-34.7287691577975,2.77656825632078,306.981356630072));
#14712=CARTESIAN_POINT('Ctrl Pts',(-34.8168085942416,2.74572771601869,306.986400268275));
#14713=CARTESIAN_POINT('Ctrl Pts',(-34.9032976151997,2.71072455764508,306.991443906477));
#14714=CARTESIAN_POINT('Ctrl Pts',(-34.9878280273348,2.67175534835848,306.99648754468));
#14715=CARTESIAN_POINT('Ctrl Pts',(-35.0724953127383,2.63272303937902,307.001539349639));
#14716=CARTESIAN_POINT('Ctrl Pts',(-35.1551972643274,2.58971206366467,307.006591154598));
#14717=CARTESIAN_POINT('Ctrl Pts',(-35.2355512495486,2.54296440489852,307.011642959557));
#14718=CARTESIAN_POINT('Ctrl Pts',(-35.2762260161533,2.51930098479069,307.014200156777));
#14719=CARTESIAN_POINT('Ctrl Pts',(-35.3162996289194,2.49468078638073,307.016757353997));
#14720=CARTESIAN_POINT('Ctrl Pts',(-35.3557255949467,2.46913920544158,307.019314551217));
#14721=CARTESIAN_POINT('Ctrl Pts',(-35.4335843309677,2.41869947223314,307.02436452623));
#14722=CARTESIAN_POINT('Ctrl Pts',(-35.5091953622117,2.364482524689,307.029414501244));
#14723=CARTESIAN_POINT('Ctrl Pts',(-35.5821689169263,2.30671519912427,307.034464476257));
#14724=CARTESIAN_POINT('Ctrl Pts',(-35.6550418028966,2.24902756495117,307.03950748471));
#14725=CARTESIAN_POINT('Ctrl Pts',(-35.7252840966099,2.18779955876853,307.044550493164));
#14726=CARTESIAN_POINT('Ctrl Pts',(-35.7925338978758,2.12330192133702,307.049593501617));
#14727=CARTESIAN_POINT('Ctrl Pts',(-35.8597117582939,2.05887328061074,307.054631115284));
#14728=CARTESIAN_POINT('Ctrl Pts',(-35.9239031698351,1.99118226687543,307.059668728952));
#14729=CARTESIAN_POINT('Ctrl Pts',(-35.9847791895293,1.92053990603867,307.064706342619));
#14730=CARTESIAN_POINT('Ctrl Pts',(-36.0456114286456,1.84994834949884,307.069740333355));
#14731=CARTESIAN_POINT('Ctrl Pts',(-36.1031327255531,1.7764100005162,307.07477432409));
#14732=CARTESIAN_POINT('Ctrl Pts',(-36.1570516650408,1.70027200002884,307.079808314826));
#14733=CARTESIAN_POINT('Ctrl Pts',(-36.2109510990481,1.62416154289233,307.084840484487));
#14734=CARTESIAN_POINT('Ctrl Pts',(-36.2612505077187,1.54545366506143,307.089872654149));
#14735=CARTESIAN_POINT('Ctrl Pts',(-36.3077000371575,1.46452694237562,307.09490482381));
#14736=CARTESIAN_POINT('Ctrl Pts',(-36.3541457898697,1.38360679969419,307.099936584315));
#14737=CARTESIAN_POINT('Ctrl Pts',(-36.3967420645186,1.30046855666009,307.104968344819));
#14738=CARTESIAN_POINT('Ctrl Pts',(-36.4352840609986,1.21551700022649,307.110000105324));
#14739=CARTESIAN_POINT('Ctrl Pts',(-36.4738337325948,1.13054852684173,307.115032867836));
#14740=CARTESIAN_POINT('Ctrl Pts',(-36.5083273392784,1.04376642805243,307.120065630348));
#14741=CARTESIAN_POINT('Ctrl Pts',(-36.5386079542234,0.955596086190086,
307.125098392859));
#14742=CARTESIAN_POINT('Ctrl Pts',(-36.5689218711038,0.86732877657978,307.130136690289));
#14743=CARTESIAN_POINT('Ctrl Pts',(-36.5950134032165,0.777670597661236,
307.135174987719));
#14744=CARTESIAN_POINT('Ctrl Pts',(-36.616775416527,0.6870624291343,307.140213285149));
#14745=CARTESIAN_POINT('Ctrl Pts',(-36.6385508920485,0.596398209438501,
307.145254699323));
#14746=CARTESIAN_POINT('Ctrl Pts',(-36.655991433999,0.50478326675529,307.150296113497));
#14747=CARTESIAN_POINT('Ctrl Pts',(-36.6690413856439,0.412666849959389,
307.155337527671));
#14748=CARTESIAN_POINT('Ctrl Pts',(-36.6821123812078,0.32040188928585,307.160387071462));
#14749=CARTESIAN_POINT('Ctrl Pts',(-36.6907786114471,0.227634282353497,
307.165436615253));
#14750=CARTESIAN_POINT('Ctrl Pts',(-36.6950364409153,0.134816343810574,
307.170486159045));
#14751=CARTESIAN_POINT('Ctrl Pts',(-36.6970988567292,0.0898570081459208,
307.172932067));
#14752=CARTESIAN_POINT('Ctrl Pts',(-36.698127730074,0.0448858346111718,
307.175377974955));
#14753=CARTESIAN_POINT('Ctrl Pts',(-36.6981270248953,-4.61727831956564E-5,
307.17782388291));
#14754=CARTESIAN_POINT('',(-36.6981258930304,0.00258108961789129,308.177823882867));
#14755=CARTESIAN_POINT('Ctrl Pts',(-36.6981270248952,-4.61761837817898E-5,
307.177823883095));
#14756=CARTESIAN_POINT('Ctrl Pts',(-36.6981269862627,-0.00250755018580523,
307.177957869859));
#14757=CARTESIAN_POINT('Ctrl Pts',(-36.6981238587313,-0.00496892131678009,
307.178091856623));
#14758=CARTESIAN_POINT('Ctrl Pts',(-36.6981176423178,-0.00743028464312453,
307.178225843386));
#14759=CARTESIAN_POINT('Ctrl Pts',(-36.6978832382483,-0.100241611014921,
307.183278120355));
#14760=CARTESIAN_POINT('Ctrl Pts',(-36.6932522120412,-0.193208428131717,
307.188330397323));
#14761=CARTESIAN_POINT('Ctrl Pts',(-36.6842043299577,-0.285879865852879,
307.193382674291));
#14762=CARTESIAN_POINT('Ctrl Pts',(-36.6751689265795,-0.378423492497563,
307.198427983234));
#14763=CARTESIAN_POINT('Ctrl Pts',(-36.661728815025,-0.470672110951617,
307.203473292176));
#14764=CARTESIAN_POINT('Ctrl Pts',(-36.6439157644718,-0.562174525986155,
307.208518601119));
#14765=CARTESIAN_POINT('Ctrl Pts',(-36.6261217774649,-0.653579015035336,
307.213558510567));
#14766=CARTESIAN_POINT('Ctrl Pts',(-36.603964237949,-0.744238454251292,
307.218598420014));
#14767=CARTESIAN_POINT('Ctrl Pts',(-36.5775266277404,-0.833707552508677,
307.223638329461));
#14768=CARTESIAN_POINT('Ctrl Pts',(-36.55110807465,-0.923112158432051,307.228674605973));
#14769=CARTESIAN_POINT('Ctrl Pts',(-36.520415708702,-1.01132770404676,307.233710882484));
#14770=CARTESIAN_POINT('Ctrl Pts',(-36.4855836934334,-1.09792089721922,
307.238747158995));
#14771=CARTESIAN_POINT('Ctrl Pts',(-36.4507643439771,-1.18448260289011,
307.243781604188));
#14772=CARTESIAN_POINT('Ctrl Pts',(-36.411808501228,-1.26942271632916,307.24881604938));
#14773=CARTESIAN_POINT('Ctrl Pts',(-36.3688992618611,-1.35232586296131,
307.253850494572));
#14774=CARTESIAN_POINT('Ctrl Pts',(-36.3259936217126,-1.4352220556942,307.258884517476));
#14775=CARTESIAN_POINT('Ctrl Pts',(-36.2791354486352,-1.51608122687307,
307.26391854038));
#14776=CARTESIAN_POINT('Ctrl Pts',(-36.2285542751424,-1.59451167886186,
307.268952563284));
#14777=CARTESIAN_POINT('Ctrl Pts',(-36.1779631946911,-1.67295749244054,
307.273987572165));
#14778=CARTESIAN_POINT('Ctrl Pts',(-36.1236479067135,-1.74897326897108,
307.279022581046));
#14779=CARTESIAN_POINT('Ctrl Pts',(-36.0658811896667,-1.82219639446329,
307.284057589926));
#14780=CARTESIAN_POINT('Ctrl Pts',(-36.0080509985243,-1.8954999775598,307.289098131277));
#14781=CARTESIAN_POINT('Ctrl Pts',(-35.9467620837555,-1.96600443507194,
307.294138672628));
#14782=CARTESIAN_POINT('Ctrl Pts',(-35.8823272320804,-2.03338060394674,
307.299179213979));
#14783=CARTESIAN_POINT('Ctrl Pts',(-35.8178527926249,-2.10079816770187,
307.30422285216));
#14784=CARTESIAN_POINT('Ctrl Pts',(-35.7502288901532,-2.16508331068846,
307.309266490342));
#14785=CARTESIAN_POINT('Ctrl Pts',(-35.6798032434156,-2.22594559854757,
307.314310128524));
#14786=CARTESIAN_POINT('Ctrl Pts',(-35.6092635621247,-2.28690643578653,
307.319361933461));
#14787=CARTESIAN_POINT('Ctrl Pts',(-35.535913428861,-2.34443307945525,307.324413738398));
#14788=CARTESIAN_POINT('Ctrl Pts',(-35.4601313513528,-2.39827714341962,
307.329465543335));
#14789=CARTESIAN_POINT('Ctrl Pts',(-35.4217708575259,-2.42553272879326,
307.332022740742));
#14790=CARTESIAN_POINT('Ctrl Pts',(-35.3827876459725,-2.45184542834557,
307.334579938149));
#14791=CARTESIAN_POINT('Ctrl Pts',(-35.3432331652808,-2.47718753837912,
307.337137135556));
#14792=CARTESIAN_POINT('Ctrl Pts',(-35.2650850369469,-2.52725616353908,
307.342189412508));
#14793=CARTESIAN_POINT('Ctrl Pts',(-35.1844250303688,-2.57371301198807,
307.34724168946));
#14794=CARTESIAN_POINT('Ctrl Pts',(-35.101621207914,-2.61629688767116,307.352293966412));
#14795=CARTESIAN_POINT('Ctrl Pts',(-35.0189315872691,-2.65882203230136,
307.357339275338));
#14796=CARTESIAN_POINT('Ctrl Pts',(-34.9341044177683,-2.69748461708392,
307.362384584264));
#14797=CARTESIAN_POINT('Ctrl Pts',(-34.8475361993156,-2.73206698577871,
307.367429893189));
#14798=CARTESIAN_POINT('Ctrl Pts',(-34.7610606262675,-2.76661234438371,
307.37246980262));
#14799=CARTESIAN_POINT('Ctrl Pts',(-34.6728481181416,-2.79708600235726,
307.377509712051));
#14800=CARTESIAN_POINT('Ctrl Pts',(-34.5833182186416,-2.82331697292174,
307.382549621482));
#14801=CARTESIAN_POINT('Ctrl Pts',(-34.4938528553049,-2.84952903532027,
307.387585897976));
#14802=CARTESIAN_POINT('Ctrl Pts',(-34.4030724132053,-2.87150436450133,
307.39262217447));
#14803=CARTESIAN_POINT('Ctrl Pts',(-34.3114137978876,-2.88912107744591,
307.397658450965));
#14804=CARTESIAN_POINT('Ctrl Pts',(-34.2197885119895,-2.90673138450255,
307.40269289614));
#14805=CARTESIAN_POINT('Ctrl Pts',(-34.1272861230806,-2.91998614013724,
307.407727341315));
#14806=CARTESIAN_POINT('Ctrl Pts',(-34.034354976131,-2.9288143005921,307.412761786491));
#14807=CARTESIAN_POINT('Ctrl Pts',(-33.9414316242277,-2.9376417205426,307.417795809378));
#14808=CARTESIAN_POINT('Ctrl Pts',(-33.8480800280715,-2.94204324171661,
307.422829832265));
#14809=CARTESIAN_POINT('Ctrl Pts',(-33.7547537779637,-2.94199967950234,
307.427863855152));
#14810=CARTESIAN_POINT('Ctrl Pts',(-33.6614092487365,-2.94195610875587,
307.432898864016));
#14811=CARTESIAN_POINT('Ctrl Pts',(-33.5680905196465,-2.93746572613335,
307.437933872879));
#14812=CARTESIAN_POINT('Ctrl Pts',(-33.4752501536014,-2.92856145282434,
307.442968881743));
#14813=CARTESIAN_POINT('Ctrl Pts',(-33.3823077745167,-2.91964739549547,
307.448009423077));
#14814=CARTESIAN_POINT('Ctrl Pts',(-33.2898452505994,-2.90630980881408,
307.453049964411));
#14815=CARTESIAN_POINT('Ctrl Pts',(-33.1983086925367,-2.88863336331915,
307.458090505745));
#14816=CARTESIAN_POINT('Ctrl Pts',(-33.1067158958218,-2.87094605768821,
307.46313414391));
#14817=CARTESIAN_POINT('Ctrl Pts',(-33.0160506289026,-2.84891469112421,
307.468177782075));
#14818=CARTESIAN_POINT('Ctrl Pts',(-32.9267453643008,-2.82267427459644,
307.47322142024));
#14819=CARTESIAN_POINT('Ctrl Pts',(-32.8372954949032,-2.79639136908337,
307.47827322516));
#14820=CARTESIAN_POINT('Ctrl Pts',(-32.7492104433979,-2.76588595274889,
307.483325030081));
#14821=CARTESIAN_POINT('Ctrl Pts',(-32.6629040097661,-2.73134169198941,
307.488376835001));
#14822=CARTESIAN_POINT('Ctrl Pts',(-32.6192161385537,-2.71385556550174,
307.490934032576));
#14823=CARTESIAN_POINT('Ctrl Pts',(-32.5759836400009,-2.69533529825264,
307.49349123015));
#14824=CARTESIAN_POINT('Ctrl Pts',(-32.5332576670678,-2.6758091360933,307.496048427725));
#14825=CARTESIAN_POINT('Ctrl Pts',(-32.4488435998329,-2.6372311318443,307.50110070467));
#14826=CARTESIAN_POINT('Ctrl Pts',(-32.3661053390023,-2.59458543339677,
307.506152981615));
#14827=CARTESIAN_POINT('Ctrl Pts',(-32.2854617960258,-2.54803998860467,
307.511205258559));
#14828=CARTESIAN_POINT('Ctrl Pts',(-32.2049294754365,-2.50155873860477,
307.516250567478));
#14829=CARTESIAN_POINT('Ctrl Pts',(-32.1264865133108,-2.45118865011795,
307.521295876397));
#14830=CARTESIAN_POINT('Ctrl Pts',(-32.0505306211471,-2.3971451575333,307.526341185316));
#14831=CARTESIAN_POINT('Ctrl Pts',(-31.9746560170669,-2.34315950235686,
307.531381094739));
#14832=CARTESIAN_POINT('Ctrl Pts',(-31.9012635525235,-2.28550851326651,
307.536421004163));
#14833=CARTESIAN_POINT('Ctrl Pts',(-31.8307241869542,-2.22445227196567,
307.541460913586));
#14834=CARTESIAN_POINT('Ctrl Pts',(-31.7602356685354,-2.16344004205998,
307.546497190073));
#14835=CARTESIAN_POINT('Ctrl Pts',(-31.6925964962286,-2.09902772875402,
307.55153346656));
#14836=CARTESIAN_POINT('Ctrl Pts',(-31.6281457537451,-2.03151660295753,
307.556569743047));
#14837=CARTESIAN_POINT('Ctrl Pts',(-31.5637184472036,-1.96403002593684,
307.561604188215));
#14838=CARTESIAN_POINT('Ctrl Pts',(-31.5024775736843,-1.89344719596045,
307.566638633383));
#14839=CARTESIAN_POINT('Ctrl Pts',(-31.4447256747144,-1.82010653443884,
307.571673078551));
#14840=CARTESIAN_POINT('Ctrl Pts',(-31.3869786199636,-1.74677202471912,
307.57670710143));
#14841=CARTESIAN_POINT('Ctrl Pts',(-31.332720232598,-1.67068049253143,307.581741124309));
#14842=CARTESIAN_POINT('Ctrl Pts',(-31.2822122999425,-1.59220285512531,
307.586775147189));
#14843=CARTESIAN_POINT('Ctrl Pts',(-31.2316944746746,-1.51370984688898,
307.591810156045));
#14844=CARTESIAN_POINT('Ctrl Pts',(-31.1849288030875,-1.4328301790294,307.596845164901));
#14845=CARTESIAN_POINT('Ctrl Pts',(-31.1421327137115,-1.34996212510011,
307.601880173757));
#14846=CARTESIAN_POINT('Ctrl Pts',(-31.0992895999725,-1.2670030157144,307.606920715083));
#14847=CARTESIAN_POINT('Ctrl Pts',(-31.0604249792384,-1.18205155439716,
307.611961256409));
#14848=CARTESIAN_POINT('Ctrl Pts',(-31.0257092828616,-1.09552861761311,
307.617001797735));
#14849=CARTESIAN_POINT('Ctrl Pts',(-30.9909722576959,-1.00895252246989,
307.622045435892));
#14850=CARTESIAN_POINT('Ctrl Pts',(-30.9603893770265,-0.920803449160516,
307.627089074049));
#14851=CARTESIAN_POINT('Ctrl Pts',(-30.9340813675908,-0.831518073191303,
307.632132712206));
#14852=CARTESIAN_POINT('Ctrl Pts',(-30.9077307597221,-0.742088124630835,
307.637184517118));
#14853=CARTESIAN_POINT('Ctrl Pts',(-30.8856689469274,-0.651518631324878,
307.64223632203));
#14854=CARTESIAN_POINT('Ctrl Pts',(-30.8679656412477,-0.560256923129221,
307.647288126943));
#14855=CARTESIAN_POINT('Ctrl Pts',(-30.859004319013,-0.514060716068839,
307.649845324593));
#14856=CARTESIAN_POINT('Ctrl Pts',(-30.8511589651056,-0.467687234591618,
307.652402522244));
#14857=CARTESIAN_POINT('Ctrl Pts',(-30.8444335387786,-0.42119477774019,
307.654959719894));
#14858=CARTESIAN_POINT('Ctrl Pts',(-30.8311460572966,-0.329339238860322,
307.660011996846));
#14859=CARTESIAN_POINT('Ctrl Pts',(-30.8221856536612,-0.236689432625149,
307.665064273798));
#14860=CARTESIAN_POINT('Ctrl Pts',(-30.8176380219122,-0.143688472809013,
307.67011655075));
#14861=CARTESIAN_POINT('Ctrl Pts',(-30.8130966621898,-0.0508157785451592,
307.675161859676));
#14862=CARTESIAN_POINT('Ctrl Pts',(-30.8129560021499,0.0424066670474889,
307.680207168603));
#14863=CARTESIAN_POINT('Ctrl Pts',(-30.8172503349368,0.135527853555428,
307.685252477529));
#14864=CARTESIAN_POINT('Ctrl Pts',(-30.8215400719239,0.228549381663997,
307.69029238696));
#14865=CARTESIAN_POINT('Ctrl Pts',(-30.8302553473273,0.321469424684481,
307.695332296391));
#14866=CARTESIAN_POINT('Ctrl Pts',(-30.8433784332003,0.413835280598431,
307.700372205822));
#14867=CARTESIAN_POINT('Ctrl Pts',(-30.8564920595112,0.50613455609483,307.705408482316));
#14868=CARTESIAN_POINT('Ctrl Pts',(-30.8740071186566,0.597879999925961,
307.710444758811));
#14869=CARTESIAN_POINT('Ctrl Pts',(-30.8958539937072,0.68862339851713,307.715481035305));
#14870=CARTESIAN_POINT('Ctrl Pts',(-30.9176929246743,0.77933380048399,307.72051548048));
#14871=CARTESIAN_POINT('Ctrl Pts',(-30.9438604384449,0.869042449589275,
307.725549925656));
#14872=CARTESIAN_POINT('Ctrl Pts',(-30.9742358969099,0.957311730848763,
307.730584370831));
#14873=CARTESIAN_POINT('Ctrl Pts',(-31.0046088074872,1.04557360809749,307.735618393718));
#14874=CARTESIAN_POINT('Ctrl Pts',(-31.0391888162568,1.13239593752782,307.740652416605));
#14875=CARTESIAN_POINT('Ctrl Pts',(-31.0778058956517,1.21735776446638,307.745686439492));
#14876=CARTESIAN_POINT('Ctrl Pts',(-31.1164305386866,1.30233623224597,307.750721448356));
#14877=CARTESIAN_POINT('Ctrl Pts',(-31.1590936385486,1.38545306956626,307.75575645722));
#14878=CARTESIAN_POINT('Ctrl Pts',(-31.2055781465145,1.46630979576026,307.760791466084));
#14879=CARTESIAN_POINT('Ctrl Pts',(-31.2521137316798,1.54725536736323,307.765832007417));
#14880=CARTESIAN_POINT('Ctrl Pts',(-31.3024788848182,1.62593548491534,307.770872548751));
#14881=CARTESIAN_POINT('Ctrl Pts',(-31.356412103035,1.70197893408303,307.775913090085));
#14882=CARTESIAN_POINT('Ctrl Pts',(-31.4103784569904,1.77806910317456,307.78095672825));
#14883=CARTESIAN_POINT('Ctrl Pts',(-31.4679169664322,1.85151902945579,307.786000366414));
#14884=CARTESIAN_POINT('Ctrl Pts',(-31.5287259275976,1.92199072582133,307.791044004579));
#14885=CARTESIAN_POINT('Ctrl Pts',(-31.5896333517975,1.99257653130713,307.7960958095));
#14886=CARTESIAN_POINT('Ctrl Pts',(-31.6538214941681,2.06017415778127,307.80114761442));
#14887=CARTESIAN_POINT('Ctrl Pts',(-31.7209520654008,2.12448273298979,307.80619941934));
#14888=CARTESIAN_POINT('Ctrl Pts',(-31.754933214046,2.15703540181405,307.808756616914));
#14889=CARTESIAN_POINT('Ctrl Pts',(-31.7896677842723,2.18874594992559,307.811313814489));
#14890=CARTESIAN_POINT('Ctrl Pts',(-31.8251089117024,2.21957947483792,307.813871012063));
#14891=CARTESIAN_POINT('Ctrl Pts',(-31.8951302479454,2.28049753168308,307.818923289013));
#14892=CARTESIAN_POINT('Ctrl Pts',(-31.9681627809449,2.33820822865134,307.823975565963));
#14893=CARTESIAN_POINT('Ctrl Pts',(-32.043880421301,2.3923995417236,307.829027842913));
#14894=CARTESIAN_POINT('Ctrl Pts',(-32.1194936330039,2.44651611493576,307.834073151837));
#14895=CARTESIAN_POINT('Ctrl Pts',(-32.1977842350866,2.49712269321824,307.839118460761));
#14896=CARTESIAN_POINT('Ctrl Pts',(-32.2783916616912,2.5439461856072,307.844163769685));
#14897=CARTESIAN_POINT('Ctrl Pts',(-32.3589128221362,2.59071956744134,307.849203679114));
#14898=CARTESIAN_POINT('Ctrl Pts',(-32.4417454967018,2.63371768876346,307.854243588543));
#14899=CARTESIAN_POINT('Ctrl Pts',(-32.5264995233976,2.6727102736117,307.859283497971));
#14900=CARTESIAN_POINT('Ctrl Pts',(-32.6111924565383,2.71167475129234,307.864319774464));
#14901=CARTESIAN_POINT('Ctrl Pts',(-32.6978035865456,2.74663924631596,307.869356050956));
#14902=CARTESIAN_POINT('Ctrl Pts',(-32.7859184220596,2.77741953371839,307.874392327449));
#14903=CARTESIAN_POINT('Ctrl Pts',(-32.8740012167619,2.80818862861977,307.879426772622));
#14904=CARTESIAN_POINT('Ctrl Pts',(-32.9635862117413,2.83477639213306,307.884461217795));
#14905=CARTESIAN_POINT('Ctrl Pts',(-33.0542401927121,2.8570472299735,307.889495662968));
#14906=CARTESIAN_POINT('Ctrl Pts',(-33.1448865696438,2.87931619974021,307.894529685853));
#14907=CARTESIAN_POINT('Ctrl Pts',(-33.2366013228173,2.89726885796858,307.899563708738));
#14908=CARTESIAN_POINT('Ctrl Pts',(-33.328938494487,2.91082015232443,307.904597731623));
#14909=CARTESIAN_POINT('Ctrl Pts',(-33.4212937515515,2.92437410087149,307.909632740484));
#14910=CARTESIAN_POINT('Ctrl Pts',(-33.5142712296474,2.93352490934955,307.914667749346));
#14911=CARTESIAN_POINT('Ctrl Pts',(-33.6074183974593,2.93823922511738,307.919702758207));
#14912=CARTESIAN_POINT('Ctrl Pts',(-33.7006679154236,2.94295872097761,307.924743299539));
#14913=CARTESIAN_POINT('Ctrl Pts',(-33.7940870509152,2.94323197091793,307.929783840871));
#14914=CARTESIAN_POINT('Ctrl Pts',(-33.8872221179377,2.93907775954894,307.934824382202));
#14915=CARTESIAN_POINT('Ctrl Pts',(-33.9804144057108,2.93492099589646,307.939868020365));
#14916=CARTESIAN_POINT('Ctrl Pts',(-34.0733218355228,2.92633139648949,307.944911658527));
#14917=CARTESIAN_POINT('Ctrl Pts',(-34.1654968812254,2.91337953604142,307.94995529669));
#14918=CARTESIAN_POINT('Ctrl Pts',(-34.2578211785276,2.90040670369281,307.955007101608));
#14919=CARTESIAN_POINT('Ctrl Pts',(-34.3494102882879,2.88305759155798,307.960058906526));
#14920=CARTESIAN_POINT('Ctrl Pts',(-34.4398280703308,2.86145363075585,307.965110711444));
#14921=CARTESIAN_POINT('Ctrl Pts',(-34.4855970852982,2.85051781721379,307.96766790904));
#14922=CARTESIAN_POINT('Ctrl Pts',(-34.5310662230126,2.83849256113043,307.970225106637));
#14923=CARTESIAN_POINT('Ctrl Pts',(-34.5761807616741,2.82539835587645,307.972782304233));
#14924=CARTESIAN_POINT('Ctrl Pts',(-34.6653139378073,2.7995280236542,307.977834581183));
#14925=CARTESIAN_POINT('Ctrl Pts',(-34.7533817034997,2.76938927675325,307.982886858132));
#14926=CARTESIAN_POINT('Ctrl Pts',(-34.8399451512711,2.73508725084313,307.987939135081));
#14927=CARTESIAN_POINT('Ctrl Pts',(-34.9263892120112,2.70083253378156,307.992984444005));
#14928=CARTESIAN_POINT('Ctrl Pts',(-35.0113326681612,2.66242610990136,307.998029752928));
#14929=CARTESIAN_POINT('Ctrl Pts',(-35.0943506689344,2.62002318300898,308.003075061852));
#14930=CARTESIAN_POINT('Ctrl Pts',(-35.1772798237484,2.57766563577736,308.00811497128));
#14931=CARTESIAN_POINT('Ctrl Pts',(-35.258287225477,2.53132028783189,308.013154880708));
#14932=CARTESIAN_POINT('Ctrl Pts',(-35.336967986493,2.48119041092786,308.018194790136));
#14933=CARTESIAN_POINT('Ctrl Pts',(-35.4155920317679,2.43109666932659,308.023231066628));
#14934=CARTESIAN_POINT('Ctrl Pts',(-35.4918923962477,2.37722405910758,308.02826734312));
#14935=CARTESIAN_POINT('Ctrl Pts',(-35.5654897282066,2.31982124509135,308.033303619612));
#14936=CARTESIAN_POINT('Ctrl Pts',(-35.6390602982899,2.262439304209,308.038338064784));
#14937=CARTESIAN_POINT('Ctrl Pts',(-35.7099294385199,2.20152998262855,308.043372509957));
#14938=CARTESIAN_POINT('Ctrl Pts',(-35.7777485380565,2.13738402234807,308.04840695513));
#14939=CARTESIAN_POINT('Ctrl Pts',(-35.8455619489394,2.07324344261896,308.053440978014));
#14940=CARTESIAN_POINT('Ctrl Pts',(-35.9103255051623,2.00586706938051,308.058475000898));
#14941=CARTESIAN_POINT('Ctrl Pts',(-35.9717261818855,1.93558373033819,308.063509023782));
#14942=CARTESIAN_POINT('Ctrl Pts',(-36.0331388847023,1.86528662542124,308.068544032643));
#14943=CARTESIAN_POINT('Ctrl Pts',(-36.0911871079274,1.79208175872787,308.073579041504));
#14944=CARTESIAN_POINT('Ctrl Pts',(-36.1455977275192,1.71633148401857,308.078614050365));
#14945=CARTESIAN_POINT('Ctrl Pts',(-36.2000681335256,1.64049797487165,308.083654591696));
#14946=CARTESIAN_POINT('Ctrl Pts',(-36.2508926978361,1.56211383615403,308.088695133027));
#14947=CARTESIAN_POINT('Ctrl Pts',(-36.2978414998532,1.48157062930902,308.093735674358));
#14948=CARTESIAN_POINT('Ctrl Pts',(-36.3448191464911,1.4009779379584,308.09877931252));
#14949=CARTESIAN_POINT('Ctrl Pts',(-36.387916085266,1.31822393141601,308.103822950682));
#14950=CARTESIAN_POINT('Ctrl Pts',(-36.4269492686713,1.23372304188852,308.108866588844));
#14951=CARTESIAN_POINT('Ctrl Pts',(-36.4660456553548,1.14908532690217,308.113918393761));
#14952=CARTESIAN_POINT('Ctrl Pts',(-36.5010649836003,1.06269549320563,308.118970198679));
#14953=CARTESIAN_POINT('Ctrl Pts',(-36.5318731245027,0.974985944783638,
308.124022003596));
#14954=CARTESIAN_POINT('Ctrl Pts',(-36.5474680465801,0.930587823604574,
308.126579201198));
#14955=CARTESIAN_POINT('Ctrl Pts',(-36.5619847260853,0.885851761033045,
308.1291363988));
#14956=CARTESIAN_POINT('Ctrl Pts',(-36.5754107538507,0.84083485756132,308.131693596402));
#14957=CARTESIAN_POINT('Ctrl Pts',(-36.6081304217728,0.731127194340305,
308.137925570431));
#14958=CARTESIAN_POINT('Ctrl Pts',(-36.6344647399623,0.619433443808255,
308.144157544461));
#14959=CARTESIAN_POINT('Ctrl Pts',(-36.6542128972751,0.506421048548363,
308.15038951849));
#14960=CARTESIAN_POINT('Ctrl Pts',(-36.6736758184333,0.395040968674961,
308.156531479852));
#14961=CARTESIAN_POINT('Ctrl Pts',(-36.6867414406795,0.282380013901316,
308.162673441214));
#14962=CARTESIAN_POINT('Ctrl Pts',(-36.6932633563957,0.169098114443563,
308.168815402576));
#14963=CARTESIAN_POINT('Ctrl Pts',(-36.6964519441951,0.113714190729772,
308.17181822934));
#14964=CARTESIAN_POINT('Ctrl Pts',(-36.6980771128039,0.0581821699086846,
308.174821056104));
#14965=CARTESIAN_POINT('Ctrl Pts',(-36.6981258930304,0.00258108961789325,
308.177823882867));
#14966=CARTESIAN_POINT('',(-36.6981267404242,-0.00129458858357652,309.177823882939));
#14967=CARTESIAN_POINT('Ctrl Pts',(-36.6981258930311,0.00258108883062432,
308.17782388291));
#14968=CARTESIAN_POINT('Ctrl Pts',(-36.6982071222146,-0.0900062577063865,
308.182824213132));
#14969=CARTESIAN_POINT('Ctrl Pts',(-36.6939133701504,-0.182678244833167,
308.187824543354));
#14970=CARTESIAN_POINT('Ctrl Pts',(-36.6852474248329,-0.274986699299511,
308.192824873577));
#14971=CARTESIAN_POINT('Ctrl Pts',(-36.6765849946573,-0.367257710958717,
308.197823175529));
#14972=CARTESIAN_POINT('Ctrl Pts',(-36.6635539350238,-0.459165034091684,
308.202821477483));
#14973=CARTESIAN_POINT('Ctrl Pts',(-36.6462090565882,-0.550263438890801,
308.207819779435));
#14974=CARTESIAN_POINT('Ctrl Pts',(-36.6288661880875,-0.641351287152581,
308.212817502182));
#14975=CARTESIAN_POINT('Ctrl Pts',(-36.6072105787433,-0.731629960143632,
308.217815224929));
#14976=CARTESIAN_POINT('Ctrl Pts',(-36.5813483292237,-0.820663502061557,
308.222812947676));
#14977=CARTESIAN_POINT('Ctrl Pts',(-36.5554815829753,-0.909712524446245,
308.227811539388));
#14978=CARTESIAN_POINT('Ctrl Pts',(-36.5254068711011,-0.99751555287184,
308.2328101311));
#14979=CARTESIAN_POINT('Ctrl Pts',(-36.491280062755,-1.08365209429455,308.237808722813));
#14980=CARTESIAN_POINT('Ctrl Pts',(-36.4571158737413,-1.16988298504469,
308.242812789713));
#14981=CARTESIAN_POINT('Ctrl Pts',(-36.4188908962147,-1.25444332544956,
308.247816856613));
#14982=CARTESIAN_POINT('Ctrl Pts',(-36.3768088818397,-1.33693328426721,
308.252820923514));
#14983=CARTESIAN_POINT('Ctrl Pts',(-36.3347011113665,-1.41947373067443,
308.25782805313));
#14984=CARTESIAN_POINT('Ctrl Pts',(-36.2887318303635,-1.4999408827083,308.262835182746));
#14985=CARTESIAN_POINT('Ctrl Pts',(-36.2391492620189,-1.57796215789515,
308.267842312361));
#14986=CARTESIAN_POINT('Ctrl Pts',(-36.1894851734741,-1.65611171022004,
308.272857674351));
#14987=CARTESIAN_POINT('Ctrl Pts',(-36.1361961997231,-1.73180699119541,
308.27787303634));
#14988=CARTESIAN_POINT('Ctrl Pts',(-36.0795719503602,-1.8047070898112,308.282888398329));
#14989=CARTESIAN_POINT('Ctrl Pts',(-36.0505318087128,-1.84209441438916,
308.285460561743));
#14990=CARTESIAN_POINT('Ctrl Pts',(-36.0206150366796,-1.87874711751359,
308.288032725157));
#14991=CARTESIAN_POINT('Ctrl Pts',(-35.989864380682,-1.91462305088542,308.290604888572));
#14992=CARTESIAN_POINT('Ctrl Pts',(-35.9294635408192,-1.98509102746083,
308.295657165522));
#14993=CARTESIAN_POINT('Ctrl Pts',(-35.8656164209312,-2.05282448081025,
308.300709442472));
#14994=CARTESIAN_POINT('Ctrl Pts',(-35.798600181269,-2.11746721508803,308.305761719422));
#14995=CARTESIAN_POINT('Ctrl Pts',(-35.7316763694166,-2.18202079505965,
308.310807028346));
#14996=CARTESIAN_POINT('Ctrl Pts',(-35.6615924401032,-2.24349182068722,
308.31585233727));
#14997=CARTESIAN_POINT('Ctrl Pts',(-35.588665333503,-2.30155759189577,308.320897646194));
#14998=CARTESIAN_POINT('Ctrl Pts',(-35.5158162735753,-2.35956122104986,
308.325937555622));
#14999=CARTESIAN_POINT('Ctrl Pts',(-35.4401304300073,-2.41416656415945,
308.330977465051));
#15000=CARTESIAN_POINT('Ctrl Pts',(-35.3619602600894,-2.46508896835582,
308.33601737448));
#15001=CARTESIAN_POINT('Ctrl Pts',(-35.2838464378613,-2.51597466596913,
308.341053650972));
#15002=CARTESIAN_POINT('Ctrl Pts',(-35.2032522198908,-2.56318245963645,
308.346089927464));
#15003=CARTESIAN_POINT('Ctrl Pts',(-35.1205608413697,-2.60646971235993,
308.351126203956));
#15004=CARTESIAN_POINT('Ctrl Pts',(-35.0378995315525,-2.6497412247293,308.356160649129));
#15005=CARTESIAN_POINT('Ctrl Pts',(-34.9531429693265,-2.68909482245021,
308.361195094303));
#15006=CARTESIAN_POINT('Ctrl Pts',(-34.8666999969098,-2.72433325322649,
308.366229539476));
#15007=CARTESIAN_POINT('Ctrl Pts',(-34.7802642753136,-2.75956872820971,
308.371263562361));
#15008=CARTESIAN_POINT('Ctrl Pts',(-34.6921428362306,-2.79068955501309,
308.376297585245));
#15009=CARTESIAN_POINT('Ctrl Pts',(-34.6027644916219,-2.81754662792797,
308.38133160813));
#15010=CARTESIAN_POINT('Ctrl Pts',(-34.513368641142,-2.84440896113784,308.386366616991));
#15011=CARTESIAN_POINT('Ctrl Pts',(-34.4227158217651,-2.86700575444401,
308.391401625853));
#15012=CARTESIAN_POINT('Ctrl Pts',(-34.3312488797567,-2.88523809285777,
308.396436634714));
#15013=CARTESIAN_POINT('Ctrl Pts',(-34.2396814338288,-2.90349046497365,
308.401477176046));
#15014=CARTESIAN_POINT('Ctrl Pts',(-34.1472985159844,-2.91736872250044,
308.406517717377));
#15015=CARTESIAN_POINT('Ctrl Pts',(-34.0545517094405,-2.92682536340492,
308.411558258709));
#15016=CARTESIAN_POINT('Ctrl Pts',(-33.9617479206874,-2.9362878143239,308.416601896871));
#15017=CARTESIAN_POINT('Ctrl Pts',(-33.868580241436,-2.94132321649804,308.421645535034));
#15018=CARTESIAN_POINT('Ctrl Pts',(-33.775501704775,-2.94193620287619,308.426689173196));
#15019=CARTESIAN_POINT('Ctrl Pts',(-33.6822724535647,-2.94255018181363,
308.431740978114));
#15020=CARTESIAN_POINT('Ctrl Pts',(-33.5891330764316,-2.93872746737211,
308.436792783032));
#15021=CARTESIAN_POINT('Ctrl Pts',(-33.4965327499461,-2.9305246650089,308.44184458795));
#15022=CARTESIAN_POINT('Ctrl Pts',(-33.4496589422253,-2.92637244875505,
308.444401785547));
#15023=CARTESIAN_POINT('Ctrl Pts',(-33.4029231193229,-2.92109872832869,
308.446958983144));
#15024=CARTESIAN_POINT('Ctrl Pts',(-33.3563824045443,-2.91471580745203,
308.449516180741));
#15025=CARTESIAN_POINT('Ctrl Pts',(-33.264431520192,-2.90210501661758,308.454568457691));
#15026=CARTESIAN_POINT('Ctrl Pts',(-33.1729129228356,-2.88511614501208,
308.459620734641));
#15027=CARTESIAN_POINT('Ctrl Pts',(-33.0822761531534,-2.86378927335172,
308.46467301159));
#15028=CARTESIAN_POINT('Ctrl Pts',(-32.9917643883678,-2.84249181539838,
308.469718320514));
#15029=CARTESIAN_POINT('Ctrl Pts',(-32.9021324631982,-2.81686834705423,
308.474763629438));
#15030=CARTESIAN_POINT('Ctrl Pts',(-32.8138233047469,-2.78701053071416,
308.479808938362));
#15031=CARTESIAN_POINT('Ctrl Pts',(-32.7256086548571,-2.75718466824303,
308.484848847791));
#15032=CARTESIAN_POINT('Ctrl Pts',(-32.6387143765055,-2.72313360655016,
308.48988875722));
#15033=CARTESIAN_POINT('Ctrl Pts',(-32.5535706483933,-2.68499947122209,
308.494928666648));
#15034=CARTESIAN_POINT('Ctrl Pts',(-32.4684882947465,-2.64689282426248,
308.499964943141));
#15035=CARTESIAN_POINT('Ctrl Pts',(-32.385154387507,-2.60470913479207,308.505001219633));
#15036=CARTESIAN_POINT('Ctrl Pts',(-32.3039804540349,-2.5586391569907,308.510037496125));
#15037=CARTESIAN_POINT('Ctrl Pts',(-32.2228360374847,-2.51258593141363,
308.515071941298));
#15038=CARTESIAN_POINT('Ctrl Pts',(-32.1438504203556,-2.46264944394638,
308.520106386471));
#15039=CARTESIAN_POINT('Ctrl Pts',(-32.0674108461888,-2.40906655502732,
308.525140831644));
#15040=CARTESIAN_POINT('Ctrl Pts',(-31.9909776837593,-2.3554881606311,308.530174854529));
#15041=CARTESIAN_POINT('Ctrl Pts',(-31.9170905033577,-2.29826422805754,
308.535208877414));
#15042=CARTESIAN_POINT('Ctrl Pts',(-31.8461068898516,-2.23767448087155,
308.540242900298));
#15043=CARTESIAN_POINT('Ctrl Pts',(-31.775109373313,-2.17707286642237,308.54527790916));
#15044=CARTESIAN_POINT('Ctrl Pts',(-31.7070168907496,-2.1131044168003,308.550312918021));
#15045=CARTESIAN_POINT('Ctrl Pts',(-31.6421524353964,-2.04608783619408,
308.555347926883));
#15046=CARTESIAN_POINT('Ctrl Pts',(-31.5772167069492,-1.97899761773754,
308.560388468214));
#15047=CARTESIAN_POINT('Ctrl Pts',(-31.5155163953081,-1.90885290243605,
308.565429009546));
#15048=CARTESIAN_POINT('Ctrl Pts',(-31.4573360056194,-1.83600758387077,
308.570469550877));
#15049=CARTESIAN_POINT('Ctrl Pts',(-31.3991198707955,-1.7631175102638,308.575513189039));
#15050=CARTESIAN_POINT('Ctrl Pts',(-31.3444282234248,-1.68752388989831,
308.580556827202));
#15051=CARTESIAN_POINT('Ctrl Pts',(-31.2935025269897,-1.60961007095846,
308.585600465364));
#15052=CARTESIAN_POINT('Ctrl Pts',(-31.2424943706916,-1.53157009247067,
308.590652270282));
#15053=CARTESIAN_POINT('Ctrl Pts',(-31.1952645638429,-1.45120279773318,
308.5957040752));
#15054=CARTESIAN_POINT('Ctrl Pts',(-31.1520087909573,-1.36891644076053,
308.600755880118));
#15055=CARTESIAN_POINT('Ctrl Pts',(-31.130112941793,-1.32726351121248,308.603313077715));
#15056=CARTESIAN_POINT('Ctrl Pts',(-31.1092346082724,-1.28511918230092,
308.605870275313));
#15057=CARTESIAN_POINT('Ctrl Pts',(-31.0893943847638,-1.24253813789563,
308.60842747291));
#15058=CARTESIAN_POINT('Ctrl Pts',(-31.0501958871502,-1.15841040784325,
308.61347974986));
#15059=CARTESIAN_POINT('Ctrl Pts',(-31.0149119140892,-1.07227495250789,
308.61853202681));
#15060=CARTESIAN_POINT('Ctrl Pts',(-30.9837522386971,-0.984531382356039,
308.62358430376));
#15061=CARTESIAN_POINT('Ctrl Pts',(-30.95263553827,-0.896908826842626,308.628629612684));
#15062=CARTESIAN_POINT('Ctrl Pts',(-30.9256319797742,-0.807682978746629,
308.633674921608));
#15063=CARTESIAN_POINT('Ctrl Pts',(-30.9029043927106,-0.717275824994563,
308.638720230532));
#15064=CARTESIAN_POINT('Ctrl Pts',(-30.8802011287366,-0.626965425081251,
308.643760139961));
#15065=CARTESIAN_POINT('Ctrl Pts',(-30.8617648481379,-0.53547666090447,
308.648800049389));
#15066=CARTESIAN_POINT('Ctrl Pts',(-30.8477090544894,-0.443248132892643,
308.653839958818));
#15067=CARTESIAN_POINT('Ctrl Pts',(-30.8336633927302,-0.351086086308426,
308.65887623531));
#15068=CARTESIAN_POINT('Ctrl Pts',(-30.8239920084853,-0.258185773713838,
308.663912511803));
#15069=CARTESIAN_POINT('Ctrl Pts',(-30.8187574246728,-0.164996453174808,
308.668948788295));
#15070=CARTESIAN_POINT('Ctrl Pts',(-30.813524744289,-0.0718410186604065,
308.673983233468));
#15071=CARTESIAN_POINT('Ctrl Pts',(-30.8127256841677,0.0216027719144301,
308.679017678641));
#15072=CARTESIAN_POINT('Ctrl Pts',(-30.8163708564597,0.114881103819076,
308.684052123814));
#15073=CARTESIAN_POINT('Ctrl Pts',(-30.8200157229953,0.208151611554675,
308.689086146699));
#15074=CARTESIAN_POINT('Ctrl Pts',(-30.8281040632372,0.301256244303458,
308.694120169584));
#15075=CARTESIAN_POINT('Ctrl Pts',(-30.8405943939178,0.393742905450918,
308.699154192469));
#15076=CARTESIAN_POINT('Ctrl Pts',(-30.8530871709866,0.486247681272225,
308.70418920133));
#15077=CARTESIAN_POINT('Ctrl Pts',(-30.8699835909764,0.578133804927413,
308.709224210192));
#15078=CARTESIAN_POINT('Ctrl Pts',(-30.8911906673589,0.668957147498904,
308.714259219053));
#15079=CARTESIAN_POINT('Ctrl Pts',(-30.912421046087,0.759880286802425,308.719299760385));
#15080=CARTESIAN_POINT('Ctrl Pts',(-30.9379714347535,0.849737880697215,
308.724340301716));
#15081=CARTESIAN_POINT('Ctrl Pts',(-30.9676984203594,0.93809909678332,308.729380843048));
#15082=CARTESIAN_POINT('Ctrl Pts',(-30.9974436697674,1.02651460063949,308.734424481211));
#15083=CARTESIAN_POINT('Ctrl Pts',(-31.0313704631717,1.11343148289836,308.739468119373));
#15084=CARTESIAN_POINT('Ctrl Pts',(-31.0692873158421,1.19843914151204,308.744511757536));
#15085=CARTESIAN_POINT('Ctrl Pts',(-31.1072655642066,1.28358444615482,308.749563562454));
#15086=CARTESIAN_POINT('Ctrl Pts',(-31.1492465701699,1.36681395929135,308.754615367372));
#15087=CARTESIAN_POINT('Ctrl Pts',(-31.1949931186672,1.44774207389058,308.75966717229));
#15088=CARTESIAN_POINT('Ctrl Pts',(-31.218149785594,1.48870746814093,308.762224369886));
#15089=CARTESIAN_POINT('Ctrl Pts',(-31.2422706200595,1.52908363206688,308.764781567483));
#15090=CARTESIAN_POINT('Ctrl Pts',(-31.2673208061614,1.56882363692934,308.767338765079));
#15091=CARTESIAN_POINT('Ctrl Pts',(-31.3168126710084,1.64733830111873,308.772391042029));
#15092=CARTESIAN_POINT('Ctrl Pts',(-31.3701123826518,1.72364961194092,308.777443318979));
#15093=CARTESIAN_POINT('Ctrl Pts',(-31.4269976224083,1.79736480014019,308.782495595929));
#15094=CARTESIAN_POINT('Ctrl Pts',(-31.4838044068807,1.87097832143846,308.787540904853));
#15095=CARTESIAN_POINT('Ctrl Pts',(-31.5441866238552,1.94200248643167,308.792586213777));
#15096=CARTESIAN_POINT('Ctrl Pts',(-31.6078777198504,2.01007186981402,308.797631522701));
#15097=CARTESIAN_POINT('Ctrl Pts',(-31.6715006535621,2.07806840526463,308.80267143213));
#15098=CARTESIAN_POINT('Ctrl Pts',(-31.7384251257932,2.14311612182166,308.807711341559));
#15099=CARTESIAN_POINT('Ctrl Pts',(-31.8083439026182,2.20488206196187,308.812751250987));
#15100=CARTESIAN_POINT('Ctrl Pts',(-31.8782122796357,2.26660347913357,308.817787527479));
#15101=CARTESIAN_POINT('Ctrl Pts',(-31.9510703391439,2.32504752859942,308.822823803972));
#15102=CARTESIAN_POINT('Ctrl Pts',(-32.0265742773425,2.37991833729216,308.827860080464));
#15103=CARTESIAN_POINT('Ctrl Pts',(-32.1020507603748,2.43476919355305,308.832894525637));
#15104=CARTESIAN_POINT('Ctrl Pts',(-32.1801708517482,2.48604912937403,308.83792897081));
#15105=CARTESIAN_POINT('Ctrl Pts',(-32.2605588027884,2.53350344225939,308.842963415984));
#15106=CARTESIAN_POINT('Ctrl Pts',(-32.3409400109021,2.58095377468577,308.847997438868));
#15107=CARTESIAN_POINT('Ctrl Pts',(-32.4235883178011,2.62457889650524,308.853031461753));
#15108=CARTESIAN_POINT('Ctrl Pts',(-32.5081012047816,2.66416882937724,308.858065484638));
#15109=CARTESIAN_POINT('Ctrl Pts',(-32.5926306446725,2.70376651643478,308.8631004935));
#15110=CARTESIAN_POINT('Ctrl Pts',(-32.6790249875007,2.73932725681039,308.868135502361));
#15111=CARTESIAN_POINT('Ctrl Pts',(-32.7668605189049,2.7706886832354,308.873170511222));
#15112=CARTESIAN_POINT('Ctrl Pts',(-32.8547925640327,2.80208456961065,308.878211052554));
#15113=CARTESIAN_POINT('Ctrl Pts',(-32.9441685397122,2.82927178191354,308.883251593885));
#15114=CARTESIAN_POINT('Ctrl Pts',(-33.0345485987383,2.85213754478671,308.888292135217));
#15115=CARTESIAN_POINT('Ctrl Pts',(-33.1249841858805,2.87501735603237,308.893335773379));
#15116=CARTESIAN_POINT('Ctrl Pts',(-33.2164246494203,2.89357034392718,308.898379411542));
#15117=CARTESIAN_POINT('Ctrl Pts',(-33.30842111349,2.90773510082476,308.903423049704));
#15118=CARTESIAN_POINT('Ctrl Pts',(-33.4005665399964,2.921922793568,308.908474854623));
#15119=CARTESIAN_POINT('Ctrl Pts',(-33.4932693230957,2.93170802346448,308.91352665954));
#15120=CARTESIAN_POINT('Ctrl Pts',(-33.586076831716,2.93708136279478,308.918578464459));
#15121=CARTESIAN_POINT('Ctrl Pts',(-33.6330555139631,2.939801319453,308.921135662055));
#15122=CARTESIAN_POINT('Ctrl Pts',(-33.680061047337,2.94139163438224,308.923692859652));
#15123=CARTESIAN_POINT('Ctrl Pts',(-33.7270351255883,2.94185615919161,308.926250057249));
#15124=CARTESIAN_POINT('Ctrl Pts',(-33.8198422098282,2.9427739247917,308.931302334199));
#15125=CARTESIAN_POINT('Ctrl Pts',(-33.9128593521207,2.93929733732222,308.936354611149));
#15126=CARTESIAN_POINT('Ctrl Pts',(-34.00563596825,2.9314005675388,308.941406888099));
#15127=CARTESIAN_POINT('Ctrl Pts',(-34.0982846282381,2.92351468886386,308.946452197023));
#15128=CARTESIAN_POINT('Ctrl Pts',(-34.1906929824389,2.91122077924747,308.951497505947));
#15129=CARTESIAN_POINT('Ctrl Pts',(-34.2824094760139,2.89454500431863,308.956542814871));
#15130=CARTESIAN_POINT('Ctrl Pts',(-34.3740278144935,2.87788707582303,308.9615827243));
#15131=CARTESIAN_POINT('Ctrl Pts',(-34.4649553293214,2.85685668210224,308.966622633728));
#15132=CARTESIAN_POINT('Ctrl Pts',(-34.5547457273513,2.83153177073226,308.971662543157));
#15133=CARTESIAN_POINT('Ctrl Pts',(-34.6444714014394,2.80622511441097,308.976698819649));
#15134=CARTESIAN_POINT('Ctrl Pts',(-34.7330611615965,2.77663021369175,308.981735096142));
#15135=CARTESIAN_POINT('Ctrl Pts',(-34.8200800835844,2.74287584292052,308.986771372634));
#15136=CARTESIAN_POINT('Ctrl Pts',(-34.9070673632628,2.70913374610333,308.991805817807));
#15137=CARTESIAN_POINT('Ctrl Pts',(-34.9924845257453,2.67123534445613,308.99684026298));
#15138=CARTESIAN_POINT('Ctrl Pts',(-35.0759139555198,2.62935856411959,309.001874708153));
#15139=CARTESIAN_POINT('Ctrl Pts',(-35.1593363872495,2.58748529639949,309.006908731038));
#15140=CARTESIAN_POINT('Ctrl Pts',(-35.2407710208066,2.54163451293277,309.011942753923));
#15141=CARTESIAN_POINT('Ctrl Pts',(-35.319823339343,2.49203086604394,309.016976776808));
#15142=CARTESIAN_POINT('Ctrl Pts',(-35.3988911412688,2.44241750365789,309.022011785669));
#15143=CARTESIAN_POINT('Ctrl Pts',(-35.4755753254025,2.38905005447213,309.02704679453));
#15144=CARTESIAN_POINT('Ctrl Pts',(-35.5495099194493,2.33219677446405,309.032081803392));
#15145=CARTESIAN_POINT('Ctrl Pts',(-35.6235257528628,2.27528102404519,309.037122344723));
#15146=CARTESIAN_POINT('Ctrl Pts',(-35.6947856126963,2.21487206843455,309.042162886055));
#15147=CARTESIAN_POINT('Ctrl Pts',(-35.7629564783556,2.15127858404679,309.047203427386));
#15148=CARTESIAN_POINT('Ctrl Pts',(-35.8311692271447,2.08764602880179,309.052247065549));
#15149=CARTESIAN_POINT('Ctrl Pts',(-35.8962888937197,2.02082536764564,309.057290703711));
#15150=CARTESIAN_POINT('Ctrl Pts',(-35.958020749553,1.95116068710615,309.062334341874));
#15151=CARTESIAN_POINT('Ctrl Pts',(-36.0198525627897,1.88138320418158,309.067386146792));
#15152=CARTESIAN_POINT('Ctrl Pts',(-36.0782853358122,1.80875285408324,309.07243795171));
#15153=CARTESIAN_POINT('Ctrl Pts',(-36.133066002866,1.73364503192726,309.077489756628));
#15154=CARTESIAN_POINT('Ctrl Pts',(-36.1607956940189,1.69562583969093,309.080046954224));
#15155=CARTESIAN_POINT('Ctrl Pts',(-36.1875903022301,1.65697227271461,309.082604151821));
#15156=CARTESIAN_POINT('Ctrl Pts',(-36.2134214872523,1.61773543172242,309.085161349418));
#15157=CARTESIAN_POINT('Ctrl Pts',(-36.2654575656193,1.5386940973436,309.090312740437));
#15158=CARTESIAN_POINT('Ctrl Pts',(-36.313762507844,1.4570088875049,309.095464131457));
#15159=CARTESIAN_POINT('Ctrl Pts',(-36.3580634308538,1.37305897223426,309.100615522476));
#15160=CARTESIAN_POINT('Ctrl Pts',(-36.4022962455816,1.28923812164482,309.105758993742));
#15161=CARTESIAN_POINT('Ctrl Pts',(-36.4425370864889,1.20315985805626,309.110902465008));
#15162=CARTESIAN_POINT('Ctrl Pts',(-36.4785563061367,1.11523217789491,309.116045936274));
#15163=CARTESIAN_POINT('Ctrl Pts',(-36.5146083760685,1.02722430584439,309.121194098494));
#15164=CARTESIAN_POINT('Ctrl Pts',(-36.5464308897537,0.937363999677886,
309.126342260713));
#15165=CARTESIAN_POINT('Ctrl Pts',(-36.5738393479957,0.84608585042522,309.131490422933));
#15166=CARTESIAN_POINT('Ctrl Pts',(-36.6011527392662,0.755124301878006,
309.136620728614));
#15167=CARTESIAN_POINT('Ctrl Pts',(-36.6240824965273,0.662755125579855,
309.141751034295));
#15168=CARTESIAN_POINT('Ctrl Pts',(-36.6424942460327,0.569428017255287,
309.146881339976));
#15169=CARTESIAN_POINT('Ctrl Pts',(-36.6610021214227,0.475613657523854,
309.152038430465));
#15170=CARTESIAN_POINT('Ctrl Pts',(-36.6749445213043,0.380831736906949,
309.157195520954));
#15171=CARTESIAN_POINT('Ctrl Pts',(-36.6842362316534,0.28555292927936,309.162352611443));
#15172=CARTESIAN_POINT('Ctrl Pts',(-36.6935279420025,0.190274121651772,
309.167509701932));
#15173=CARTESIAN_POINT('Ctrl Pts',(-36.6981688930621,0.0944988561008657,
309.172666792421));
#15174=CARTESIAN_POINT('Ctrl Pts',(-36.6981267404244,-0.00129458804859771,
309.17782388291));
#15175=CARTESIAN_POINT('',(-36.6981263554947,-0.00198516614128411,310.177823882873));
#15176=CARTESIAN_POINT('Ctrl Pts',(-36.6981267404242,-0.00129458858357462,
309.177823882939));
#15177=CARTESIAN_POINT('Ctrl Pts',(-36.6980816154796,-0.103842668990332,
309.183344612826));
#15178=CARTESIAN_POINT('Ctrl Pts',(-36.6926705574948,-0.206216608946654,
309.188865342713));
#15179=CARTESIAN_POINT('Ctrl Pts',(-36.6819732173234,-0.307876696704694,
309.194386072601));
#15180=CARTESIAN_POINT('Ctrl Pts',(-36.6712685285798,-0.409606620186989,
309.199910594971));
#15181=CARTESIAN_POINT('Ctrl Pts',(-36.6552704312908,-0.510621430714575,
309.205435117342));
#15182=CARTESIAN_POINT('Ctrl Pts',(-36.6341091164029,-0.610395841275999,
309.210959639712));
#15183=CARTESIAN_POINT('Ctrl Pts',(-36.6128527097254,-0.710618604281967,
309.216508987417));
#15184=CARTESIAN_POINT('Ctrl Pts',(-36.5863867044715,-0.809589515636939,
309.222058335122));
#15185=CARTESIAN_POINT('Ctrl Pts',(-36.5548919122116,-0.906796067235132,
309.227607682827));
#15186=CARTESIAN_POINT('Ctrl Pts',(-36.5237434792017,-1.00293360437476,
309.233096002414));
#15187=CARTESIAN_POINT('Ctrl Pts',(-36.487676512234,-1.09734517951563,309.238584322001));
#15188=CARTESIAN_POINT('Ctrl Pts',(-36.4469105673794,-1.18955787141553,
309.244072641587));
#15189=CARTESIAN_POINT('Ctrl Pts',(-36.4093834444996,-1.27444433810589,
309.249124918537));
#15190=CARTESIAN_POINT('Ctrl Pts',(-36.3677681375394,-1.35770562351083,
309.254177195487));
#15191=CARTESIAN_POINT('Ctrl Pts',(-36.3222273810831,-1.43892076356983,
309.259229472437));
#15192=CARTESIAN_POINT('Ctrl Pts',(-36.2767494337668,-1.52002389290482,
309.264274781361));
#15193=CARTESIAN_POINT('Ctrl Pts',(-36.2273570105023,-1.59908610046198,
309.269320090285));
#15194=CARTESIAN_POINT('Ctrl Pts',(-36.1742605919241,-1.67570703100528,
309.274365399209));
#15195=CARTESIAN_POINT('Ctrl Pts',(-36.1212209971936,-1.7522459617415,309.279405308638));
#15196=CARTESIAN_POINT('Ctrl Pts',(-36.0644855379172,-1.8263484453264,309.284445218066));
#15197=CARTESIAN_POINT('Ctrl Pts',(-36.0043096707011,-1.89764032227573,
309.289485127495));
#15198=CARTESIAN_POINT('Ctrl Pts',(-35.9441771802757,-1.96888080964038,
309.294521403987));
#15199=CARTESIAN_POINT('Ctrl Pts',(-35.88060949691,-2.03731437877704,309.29955768048));
#15200=CARTESIAN_POINT('Ctrl Pts',(-35.8139036589452,-2.10259823215213,
309.304593956972));
#15201=CARTESIAN_POINT('Ctrl Pts',(-35.7472220769321,-2.16785834664556,
309.309628402145));
#15202=CARTESIAN_POINT('Ctrl Pts',(-35.6774049244454,-2.22997071025078,
309.314662847318));
#15203=CARTESIAN_POINT('Ctrl Pts',(-35.6047868410956,-2.28862860361957,
309.319697292492));
#15204=CARTESIAN_POINT('Ctrl Pts',(-35.5321748489373,-2.34728157677513,
309.324731315376));
#15205=CARTESIAN_POINT('Ctrl Pts',(-35.4567627387438,-2.40248037679104,
309.329765338261));
#15206=CARTESIAN_POINT('Ctrl Pts',(-35.3789181493797,-2.45395863198031,
309.334799361146));
#15207=CARTESIAN_POINT('Ctrl Pts',(-35.3010583131751,-2.50544696983236,
309.339834370008));
#15208=CARTESIAN_POINT('Ctrl Pts',(-35.2207654223469,-2.55321307090029,
309.344869378869));
#15209=CARTESIAN_POINT('Ctrl Pts',(-35.1384350206219,-2.59703457927538,
309.34990438773));
#15210=CARTESIAN_POINT('Ctrl Pts',(-35.0560141542123,-2.64090423874465,
309.354944929062));
#15211=CARTESIAN_POINT('Ctrl Pts',(-34.9715517007319,-2.68082044464556,
309.359985470393));
#15212=CARTESIAN_POINT('Ctrl Pts',(-34.8854663884954,-2.71660755403532,
309.365026011725));
#15213=CARTESIAN_POINT('Ctrl Pts',(-34.7993281867691,-2.7524166504738,309.370069649887));
#15214=CARTESIAN_POINT('Ctrl Pts',(-34.7115655589009,-2.78409144931857,
309.37511328805));
#15215=CARTESIAN_POINT('Ctrl Pts',(-34.6226136480587,-2.81150581228402,
309.380156926213));
#15216=CARTESIAN_POINT('Ctrl Pts',(-34.5335177045785,-2.83896456511108,
309.385208731131));
#15217=CARTESIAN_POINT('Ctrl Pts',(-34.4432290634392,-2.86214899953839,
309.390260536049));
#15218=CARTESIAN_POINT('Ctrl Pts',(-34.3521941546287,-2.88098385578317,
309.395312340967));
#15219=CARTESIAN_POINT('Ctrl Pts',(-34.3061127532644,-2.89051796288117,
309.397869538563));
#15220=CARTESIAN_POINT('Ctrl Pts',(-34.2598402376198,-2.89893838835919,
309.40042673616));
#15221=CARTESIAN_POINT('Ctrl Pts',(-34.2134348530919,-2.90624044955015,
309.402983933757));
#15222=CARTESIAN_POINT('Ctrl Pts',(-34.1217513418569,-2.92066719368881,
309.408036210707));
#15223=CARTESIAN_POINT('Ctrl Pts',(-34.029219908507,-2.93077705337543,309.413088487657));
#15224=CARTESIAN_POINT('Ctrl Pts',(-33.9362825688734,-2.93647884039788,
309.418140764607));
#15225=CARTESIAN_POINT('Ctrl Pts',(-33.8434734070486,-2.94217276359973,
309.423186073531));
#15226=CARTESIAN_POINT('Ctrl Pts',(-33.7502598909476,-2.9434706680037,309.428231382455));
#15227=CARTESIAN_POINT('Ctrl Pts',(-33.6570925705185,-2.94033266430425,
309.433276691379));
#15228=CARTESIAN_POINT('Ctrl Pts',(-33.5640249578617,-2.93719801889993,
309.438316600808));
#15229=CARTESIAN_POINT('Ctrl Pts',(-33.471003884229,-2.92963691626866,309.443356510236));
#15230=CARTESIAN_POINT('Ctrl Pts',(-33.3784822368284,-2.91766146318799,
309.448396419665));
#15231=CARTESIAN_POINT('Ctrl Pts',(-33.2860272821458,-2.90569464241702,
309.453432696157));
#15232=CARTESIAN_POINT('Ctrl Pts',(-33.1940714774529,-2.8893198527529,309.458468972649));
#15233=CARTESIAN_POINT('Ctrl Pts',(-33.1030638660051,-2.86860114167639,
309.463505249142));
#15234=CARTESIAN_POINT('Ctrl Pts',(-33.0120893472565,-2.84788996445406,
309.468539694315));
#15235=CARTESIAN_POINT('Ctrl Pts',(-32.9220627695326,-2.8228381023016,309.473574139488));
#15236=CARTESIAN_POINT('Ctrl Pts',(-32.8334232116875,-2.79356075151824,
309.478608584661));
#15237=CARTESIAN_POINT('Ctrl Pts',(-32.744791088912,-2.76428585651363,309.483642607546));
#15238=CARTESIAN_POINT('Ctrl Pts',(-32.6575461764826,-2.73078631708073,
309.488676630431));
#15239=CARTESIAN_POINT('Ctrl Pts',(-32.5721115073424,-2.6932269219908,309.493710653315));
#15240=CARTESIAN_POINT('Ctrl Pts',(-32.4866601047493,-2.65566017042164,
309.498745662177));
#15241=CARTESIAN_POINT('Ctrl Pts',(-32.403020056118,-2.61403216309794,309.503780671038));
#15242=CARTESIAN_POINT('Ctrl Pts',(-32.3215925058338,-2.568554985314,309.5088156799));
#15243=CARTESIAN_POINT('Ctrl Pts',(-32.2400754829186,-2.52302783718558,
309.513856221231));
#15244=CARTESIAN_POINT('Ctrl Pts',(-32.1607761995675,-2.47364329302981,
309.518896762563));
#15245=CARTESIAN_POINT('Ctrl Pts',(-32.0840690877834,-2.42065822736906,
309.523937303894));
#15246=CARTESIAN_POINT('Ctrl Pts',(-32.0073148483313,-2.36764060850013,
309.528980942057));
#15247=CARTESIAN_POINT('Ctrl Pts',(-31.9331563038188,-2.31101833366077,
309.534024580219));
#15248=CARTESIAN_POINT('Ctrl Pts',(-31.8619351606309,-2.25108888762352,
309.539068218381));
#15249=CARTESIAN_POINT('Ctrl Pts',(-31.7905986948039,-2.19106240267938,
309.544120023299));
#15250=CARTESIAN_POINT('Ctrl Pts',(-31.7222094511841,-2.1277183573741,309.549171828217));
#15251=CARTESIAN_POINT('Ctrl Pts',(-31.657072478335,-2.06139127994748,309.554223633135));
#15252=CARTESIAN_POINT('Ctrl Pts',(-31.6241004785967,-2.02781685540956,
309.556780830732));
#15253=CARTESIAN_POINT('Ctrl Pts',(-31.5919611817867,-1.9934786133201,309.559338028329));
#15254=CARTESIAN_POINT('Ctrl Pts',(-31.5606900694731,-1.95842298117025,
309.561895225926));
#15255=CARTESIAN_POINT('Ctrl Pts',(-31.498907468028,-1.88916327183208,309.566947502876));
#15256=CARTESIAN_POINT('Ctrl Pts',(-31.4402945985846,-1.81685278188497,
309.571999779826));
#15257=CARTESIAN_POINT('Ctrl Pts',(-31.3851675091636,-1.74181370216312,
309.577052056776));
#15258=CARTESIAN_POINT('Ctrl Pts',(-31.3301164502117,-1.66687811523385,
309.5820973657));
#15259=CARTESIAN_POINT('Ctrl Pts',(-31.2785418788373,-1.58922177146578,
309.587142674624));
#15260=CARTESIAN_POINT('Ctrl Pts',(-31.2307213409938,-1.50920181880628,
309.592187983548));
#15261=CARTESIAN_POINT('Ctrl Pts',(-31.1829519807444,-1.42926750359124,
309.597227892976));
#15262=CARTESIAN_POINT('Ctrl Pts',(-31.1389288951702,-1.34697498662043,
309.602267802405));
#15263=CARTESIAN_POINT('Ctrl Pts',(-31.0988871859254,-1.26271154119455,
309.607307711834));
#15264=CARTESIAN_POINT('Ctrl Pts',(-31.0588743400925,-1.1785088356965,309.612343988326));
#15265=CARTESIAN_POINT('Ctrl Pts',(-31.0228373563694,-1.09233842570844,
309.617380264819));
#15266=CARTESIAN_POINT('Ctrl Pts',(-30.9909655909837,-1.0046124836992,309.622416541311));
#15267=CARTESIAN_POINT('Ctrl Pts',(-30.9591054149884,-0.916918441090031,
309.627450986484));
#15268=CARTESIAN_POINT('Ctrl Pts',(-30.931407600005,-0.827670407278449,
309.632485431657));
#15269=CARTESIAN_POINT('Ctrl Pts',(-30.9080131077536,-0.737299879913195,
309.63751987683));
#15270=CARTESIAN_POINT('Ctrl Pts',(-30.8846205778279,-0.646936932811046,
309.642553899715));
#15271=CARTESIAN_POINT('Ctrl Pts',(-30.8655307641165,-0.555452109481651,
309.6475879226));
#15272=CARTESIAN_POINT('Ctrl Pts',(-30.8508342484798,-0.463290277474835,
309.652621945485));
#15273=CARTESIAN_POINT('Ctrl Pts',(-30.836134854346,-0.371110394415744,
309.657656954346));
#15274=CARTESIAN_POINT('Ctrl Pts',(-30.8258305367978,-0.278253678079413,
309.662691963208));
#15275=CARTESIAN_POINT('Ctrl Pts',(-30.8199602635903,-0.185172210874213,
309.667726972069));
#15276=CARTESIAN_POINT('Ctrl Pts',(-30.8140835401238,-0.0919884657087816,
309.672767513401));
#15277=CARTESIAN_POINT('Ctrl Pts',(-30.8126506143522,0.00142007921788039,
309.677808054732));
#15278=CARTESIAN_POINT('Ctrl Pts',(-30.8156483351303,0.0945995396776959,
309.682848596064));
#15279=CARTESIAN_POINT('Ctrl Pts',(-30.8186478976619,0.187836248162711,
309.687892234226));
#15280=CARTESIAN_POINT('Ctrl Pts',(-30.8260834905748,0.280843149467654,
309.692935872389));
#15281=CARTESIAN_POINT('Ctrl Pts',(-30.837890100144,0.373171875820337,309.697979510551));
#15282=CARTESIAN_POINT('Ctrl Pts',(-30.8497158272015,0.465650102615157,
309.70303131547));
#15283=CARTESIAN_POINT('Ctrl Pts',(-30.8659266233817,0.557447525268726,
309.708083120388));
#15284=CARTESIAN_POINT('Ctrl Pts',(-30.8864064811281,0.648126529777455,
309.713134925306));
#15285=CARTESIAN_POINT('Ctrl Pts',(-30.8967732795013,0.694027774212889,
309.715692122902));
#15286=CARTESIAN_POINT('Ctrl Pts',(-30.9082331591181,0.739642688745836,
309.718249320499));
#15287=CARTESIAN_POINT('Ctrl Pts',(-30.9207663074984,0.784916301390221,
309.720806518095));
#15288=CARTESIAN_POINT('Ctrl Pts',(-30.9455281549042,0.874363761341351,
309.725858795045));
#15289=CARTESIAN_POINT('Ctrl Pts',(-30.9745713139954,0.962798880669171,
309.730911071995));
#15290=CARTESIAN_POINT('Ctrl Pts',(-31.0077961057622,1.04978148056891,309.735963348945));
#15291=CARTESIAN_POINT('Ctrl Pts',(-31.0409750743859,1.13664411534911,309.741008657869));
#15292=CARTESIAN_POINT('Ctrl Pts',(-31.0783240582896,1.22205780008977,309.746053966793));
#15293=CARTESIAN_POINT('Ctrl Pts',(-31.1196931396859,1.30559579005501,309.751099275717));
#15294=CARTESIAN_POINT('Ctrl Pts',(-31.1610179478442,1.38904437756827,309.756139185145));
#15295=CARTESIAN_POINT('Ctrl Pts',(-31.2063541059076,1.47062086428266,309.761179094574));
#15296=CARTESIAN_POINT('Ctrl Pts',(-31.2555033840231,1.54991787037215,309.766219004002));
#15297=CARTESIAN_POINT('Ctrl Pts',(-31.3046172336844,1.62915771651045,309.771255280495));
#15298=CARTESIAN_POINT('Ctrl Pts',(-31.3575385067491,1.7061209714464,309.776291556987));
#15299=CARTESIAN_POINT('Ctrl Pts',(-31.4140232667962,1.78042522578204,309.781327833479));
#15300=CARTESIAN_POINT('Ctrl Pts',(-31.4704874875374,1.85470246118713,309.786362278652));
#15301=CARTESIAN_POINT('Ctrl Pts',(-31.5305123524841,1.92632226349048,309.791396723825));
#15302=CARTESIAN_POINT('Ctrl Pts',(-31.5938114696656,1.99493243946875,309.796431168998));
#15303=CARTESIAN_POINT('Ctrl Pts',(-31.6571052773288,2.06353686043815,309.801465191883));
#15304=CARTESIAN_POINT('Ctrl Pts',(-31.7236724897918,2.12913183060961,309.806499214768));
#15305=CARTESIAN_POINT('Ctrl Pts',(-31.7931881905498,2.19140026722548,309.811533237653));
#15306=CARTESIAN_POINT('Ctrl Pts',(-31.8627175068308,2.25368089989671,309.816568246514));
#15307=CARTESIAN_POINT('Ctrl Pts',(-31.9351961271814,2.3126334089249,309.821603255375));
#15308=CARTESIAN_POINT('Ctrl Pts',(-32.0102651163,2.36798019308669,309.826638264237));
#15309=CARTESIAN_POINT('Ctrl Pts',(-32.0854165912594,2.42338779232112,309.831678805568));
#15310=CARTESIAN_POINT('Ctrl Pts',(-32.1631637584059,2.47518149408124,309.8367193469));
#15311=CARTESIAN_POINT('Ctrl Pts',(-32.243117940682,2.52312653467709,309.841759888231));
#15312=CARTESIAN_POINT('Ctrl Pts',(-32.3231212455761,2.57110103196735,309.846803526394));
#15313=CARTESIAN_POINT('Ctrl Pts',(-32.4053338738849,2.61522195079954,309.851847164556));
#15314=CARTESIAN_POINT('Ctrl Pts',(-32.4893436976716,2.65530111304727,309.856890802718));
#15315=CARTESIAN_POINT('Ctrl Pts',(-32.5734895517741,2.69544517224219,309.861942607636));
#15316=CARTESIAN_POINT('Ctrl Pts',(-32.6594380018191,2.73153423780507,309.866994412554));
#15317=CARTESIAN_POINT('Ctrl Pts',(-32.7467583422055,2.76342882334134,309.872046217472));
#15318=CARTESIAN_POINT('Ctrl Pts',(-32.7909594481981,2.77957369805941,309.87460341507));
#15319=CARTESIAN_POINT('Ctrl Pts',(-32.8355118547494,2.79464460846844,309.877160612667));
#15320=CARTESIAN_POINT('Ctrl Pts',(-32.8803586198137,2.80862843751649,309.879717810264));
#15321=CARTESIAN_POINT('Ctrl Pts',(-32.9689627533585,2.83625640699573,309.884770087214));
#15322=CARTESIAN_POINT('Ctrl Pts',(-33.059034585095,2.85973704898571,309.889822364164));
#15323=CARTESIAN_POINT('Ctrl Pts',(-33.1501500967158,2.87891576154549,309.894874641114));
#15324=CARTESIAN_POINT('Ctrl Pts',(-33.2411399431661,2.89806802310761,309.899919950038));
#15325=CARTESIAN_POINT('Ctrl Pts',(-33.3331701782177,2.91293005446495,309.904965258962));
#15326=CARTESIAN_POINT('Ctrl Pts',(-33.4258008680034,2.92339676230129,309.910010567886));
#15327=CARTESIAN_POINT('Ctrl Pts',(-33.5183324243195,2.93385226865499,309.915050477315));
#15328=CARTESIAN_POINT('Ctrl Pts',(-33.6114627190154,2.93992175154605,309.920090386743));
#15329=CARTESIAN_POINT('Ctrl Pts',(-33.704741931871,2.94155121869017,309.925130296172));
#15330=CARTESIAN_POINT('Ctrl Pts',(-33.7979539059301,2.94317951125953,309.930166572664));
#15331=CARTESIAN_POINT('Ctrl Pts',(-33.8913141418738,2.94037414181105,309.935202849157));
#15332=CARTESIAN_POINT('Ctrl Pts',(-33.9843690564791,2.93313306469104,309.940239125649));
#15333=CARTESIAN_POINT('Ctrl Pts',(-34.0773901339334,2.9258946206122,309.945273570822));
#15334=CARTESIAN_POINT('Ctrl Pts',(-34.1701056681364,2.91422370756331,309.950308015995));
#15335=CARTESIAN_POINT('Ctrl Pts',(-34.2620644833797,2.89817033461957,309.955342461169));
#15336=CARTESIAN_POINT('Ctrl Pts',(-34.3540155851347,2.88211830822978,309.960376484053));
#15337=CARTESIAN_POINT('Ctrl Pts',(-34.4452096565233,2.86168462939899,309.965410506938));
#15338=CARTESIAN_POINT('Ctrl Pts',(-34.5352041727013,2.83697070804952,309.970444529823));
#15339=CARTESIAN_POINT('Ctrl Pts',(-34.6252163154354,2.81225194616819,309.975479538684));
#15340=CARTESIAN_POINT('Ctrl Pts',(-34.7140280080785,2.78325139481781,309.980514547546));
#15341=CARTESIAN_POINT('Ctrl Pts',(-34.8012114914192,2.75012044437833,309.985549556407));
#15342=CARTESIAN_POINT('Ctrl Pts',(-34.8884907720128,2.7169530896348,309.990590097739));
#15343=CARTESIAN_POINT('Ctrl Pts',(-34.9741378561696,2.6796464345063,309.99563063907));
#15344=CARTESIAN_POINT('Ctrl Pts',(-35.0577448879104,2.6384000719419,310.000671180402));
#15345=CARTESIAN_POINT('Ctrl Pts',(-35.1414032865237,2.5971283682477,310.005714818564));
#15346=CARTESIAN_POINT('Ctrl Pts',(-35.223018749177,2.55191235351768,310.010758456727));
#15347=CARTESIAN_POINT('Ctrl Pts',(-35.3022098809528,2.50299656478496,310.015802094889));
#15348=CARTESIAN_POINT('Ctrl Pts',(-35.381529240526,2.45400157067023,310.020853899807));
#15349=CARTESIAN_POINT('Ctrl Pts',(-35.4584160664295,2.40129509363968,310.025905704725));
#15350=CARTESIAN_POINT('Ctrl Pts',(-35.5325198346268,2.34516365885654,310.030957509643));
#15351=CARTESIAN_POINT('Ctrl Pts',(-35.5700307799295,2.3167502160434,310.03351470724));
#15352=CARTESIAN_POINT('Ctrl Pts',(-35.6068291656455,2.2874598067233,310.036071904837));
#15353=CARTESIAN_POINT('Ctrl Pts',(-35.642873125783,2.25733319475707,310.038629102434));
#15354=CARTESIAN_POINT('Ctrl Pts',(-35.7130960226271,2.19863881277755,310.043611180496));
#15355=CARTESIAN_POINT('Ctrl Pts',(-35.7807203985796,2.1365446975608,310.048593258558));
#15356=CARTESIAN_POINT('Ctrl Pts',(-35.8453917268001,2.07131287035265,310.05357533662));
#15357=CARTESIAN_POINT('Ctrl Pts',(-35.9125935919664,2.00352857432506,310.05875235938));
#15358=CARTESIAN_POINT('Ctrl Pts',(-35.9766061277763,1.93235620548142,310.063929382141));
#15359=CARTESIAN_POINT('Ctrl Pts',(-36.0370672991168,1.85813763405383,310.069106404901));
#15360=CARTESIAN_POINT('Ctrl Pts',(-36.0951028747957,1.78689658093877,310.074075734631));
#15361=CARTESIAN_POINT('Ctrl Pts',(-36.149866219895,1.71284943135371,310.07904506436));
#15362=CARTESIAN_POINT('Ctrl Pts',(-36.2010742862668,1.63633642350331,310.084014394089));
#15363=CARTESIAN_POINT('Ctrl Pts',(-36.252251367175,1.5598697128711,310.088980716929));
#15364=CARTESIAN_POINT('Ctrl Pts',(-36.2998771858322,1.4809404851409,310.093947039769));
#15365=CARTESIAN_POINT('Ctrl Pts',(-36.3437102606287,1.39992035488687,310.098913362609));
#15366=CARTESIAN_POINT('Ctrl Pts',(-36.3875298767662,1.31892510133392,310.103878160573));
#15367=CARTESIAN_POINT('Ctrl Pts',(-36.4275588445785,1.2358406227864,310.108842958536));
#15368=CARTESIAN_POINT('Ctrl Pts',(-36.4636008360711,1.15106453501049,310.113807756499));
#15369=CARTESIAN_POINT('Ctrl Pts',(-36.4996425024049,1.06628921205609,310.118772509671));
#15370=CARTESIAN_POINT('Ctrl Pts',(-36.5316970872211,0.979822732429954,
310.123737262844));
#15371=CARTESIAN_POINT('Ctrl Pts',(-36.5596162898467,0.89208292402314,310.128702016016));
#15372=CARTESIAN_POINT('Ctrl Pts',(-36.5875575363704,0.804273839733983,
310.133670689161));
#15373=CARTESIAN_POINT('Ctrl Pts',(-36.6113567457612,0.715189857057896,
310.138639362306));
#15374=CARTESIAN_POINT('Ctrl Pts',(-36.6309156226946,0.625263560465722,
310.143608035451));
#15375=CARTESIAN_POINT('Ctrl Pts',(-36.6504837121961,0.535294907038126,
310.148579048927));
#15376=CARTESIAN_POINT('Ctrl Pts',(-36.665807418628,0.444483601232109,310.153550062402));
#15377=CARTESIAN_POINT('Ctrl Pts',(-36.6768400203945,0.353269868568233,
310.158521075878));
#15378=CARTESIAN_POINT('Ctrl Pts',(-36.6878871247899,0.261936233188972,
310.163498623874));
#15379=CARTESIAN_POINT('Ctrl Pts',(-36.6946318385709,0.170199571086817,
310.168476171871));
#15380=CARTESIAN_POINT('Ctrl Pts',(-36.697079495602,0.0785020201984402,
310.173453719867));
#15381=CARTESIAN_POINT('Ctrl Pts',(-36.697795822879,0.0516659659204363,
310.174910440869));
#15382=CARTESIAN_POINT('Ctrl Pts',(-36.6981444516876,0.0248332378491975,
310.176367161871));
#15383=CARTESIAN_POINT('Ctrl Pts',(-36.6981263554947,-0.00198516614128179,
310.177823882873));
#15384=CARTESIAN_POINT('',(-36.6981260264717,0.00242422262951868,311.177823882937));
#15385=CARTESIAN_POINT('Ctrl Pts',(-36.6981263554942,-0.00198516682809399,
310.17782388291));
#15386=CARTESIAN_POINT('Ctrl Pts',(-36.6980447123328,-0.122979595449192,
310.184396053475));
#15387=CARTESIAN_POINT('Ctrl Pts',(-36.690499043274,-0.243723585403416,
310.190968224039));
#15388=CARTESIAN_POINT('Ctrl Pts',(-36.6755806319958,-0.363530793885655,
310.197540394603));
#15389=CARTESIAN_POINT('Ctrl Pts',(-36.664112283041,-0.455631142144333,
310.202592671552));
#15390=CARTESIAN_POINT('Ctrl Pts',(-36.6482608242988,-0.547353585824939,
310.207644948502));
#15391=CARTESIAN_POINT('Ctrl Pts',(-36.6280607528387,-0.638248121330511,
310.212697225451));
#15392=CARTESIAN_POINT('Ctrl Pts',(-36.6078885410195,-0.729017296432616,
310.217742534374));
#15393=CARTESIAN_POINT('Ctrl Pts',(-36.5833797299021,-0.81896040242599,
310.222787843298));
#15394=CARTESIAN_POINT('Ctrl Pts',(-36.5546204763606,-0.907633408449618,
310.227833152221));
#15395=CARTESIAN_POINT('Ctrl Pts',(-36.5258920010048,-0.996211516521299,
310.232873061649));
#15396=CARTESIAN_POINT('Ctrl Pts',(-36.4929222610277,-1.08352180604662,
310.237912971077));
#15397=CARTESIAN_POINT('Ctrl Pts',(-36.4558480308637,-1.16913236713767,
310.242952880505));
#15398=CARTESIAN_POINT('Ctrl Pts',(-36.4188005250528,-1.25468121725462,
310.247989156997));
#15399=CARTESIAN_POINT('Ctrl Pts',(-36.3776545858314,-1.33853236773728,
310.253025433489));
#15400=CARTESIAN_POINT('Ctrl Pts',(-36.3325958440165,-1.42027195493082,
310.258061709981));
#15401=CARTESIAN_POINT('Ctrl Pts',(-36.2875534867145,-1.50198181951631,
310.263096155153));
#15402=CARTESIAN_POINT('Ctrl Pts',(-36.2386013676048,-1.58158125749836,
310.268130600326));
#15403=CARTESIAN_POINT('Ctrl Pts',(-36.1859715216672,-1.65868011481058,
310.273165045499));
#15404=CARTESIAN_POINT('Ctrl Pts',(-36.1333460903113,-1.73577250508494,
310.278199068383));
#15405=CARTESIAN_POINT('Ctrl Pts',(-36.0770437960919,-1.81036436490259,
310.283233091267));
#15406=CARTESIAN_POINT('Ctrl Pts',(-36.0173399019926,-1.88209466448626,
310.288267114152));
#15407=CARTESIAN_POINT('Ctrl Pts',(-35.9576243141357,-1.95383901335018,
310.293302123013));
#15408=CARTESIAN_POINT('Ctrl Pts',(-35.894506087705,-2.02272034768265,310.298337131874));
#15409=CARTESIAN_POINT('Ctrl Pts',(-35.8282998927217,-2.08841174277138,
310.303372140734));
#15410=CARTESIAN_POINT('Ctrl Pts',(-35.7620209503401,-2.15417531959619,
310.308412682066));
#15411=CARTESIAN_POINT('Ctrl Pts',(-35.6926475823017,-2.21674164717611,
310.313453223397));
#15412=CARTESIAN_POINT('Ctrl Pts',(-35.6205301230968,-2.27582184908392,
310.318493764728));
#15413=CARTESIAN_POINT('Ctrl Pts',(-35.5483683560356,-2.33493834895779,
310.32353740289));
#15414=CARTESIAN_POINT('Ctrl Pts',(-35.4734594978642,-2.39056419455085,
310.328581041052));
#15415=CARTESIAN_POINT('Ctrl Pts',(-35.3961838697211,-2.44245318213646,
310.333624679214));
#15416=CARTESIAN_POINT('Ctrl Pts',(-35.3187831154005,-2.49442618936478,
310.338676484131));
#15417=CARTESIAN_POINT('Ctrl Pts',(-35.2390083200674,-2.54265002938534,
310.343728289049));
#15418=CARTESIAN_POINT('Ctrl Pts',(-35.1572652770677,-2.58692396473389,
310.348780093967));
#15419=CARTESIAN_POINT('Ctrl Pts',(-35.1158873701716,-2.60933520252919,
310.351337291569));
#15420=CARTESIAN_POINT('Ctrl Pts',(-35.0740054704259,-2.63073510327062,
310.353894489171));
#15421=CARTESIAN_POINT('Ctrl Pts',(-35.0316740018305,-2.65110239533592,
310.356451686773));
#15422=CARTESIAN_POINT('Ctrl Pts',(-34.9480393609716,-2.69134222668754,
310.361503963723));
#15423=CARTESIAN_POINT('Ctrl Pts',(-34.8623485549746,-2.72769275884657,
310.366556240673));
#15424=CARTESIAN_POINT('Ctrl Pts',(-34.7749985594086,-2.75993927413208,
310.371608517623));
#15425=CARTESIAN_POINT('Ctrl Pts',(-34.687769035669,-2.79214131549904,310.376653826547));
#15426=CARTESIAN_POINT('Ctrl Pts',(-34.5988852827091,-2.8202504350076,310.381699135471));
#15427=CARTESIAN_POINT('Ctrl Pts',(-34.508767233588,-2.84409857719532,310.386744444395));
#15428=CARTESIAN_POINT('Ctrl Pts',(-34.4187456289057,-2.86792119707408,
310.391784353824));
#15429=CARTESIAN_POINT('Ctrl Pts',(-34.3274927808052,-2.88749179048213,
310.396824263252));
#15430=CARTESIAN_POINT('Ctrl Pts',(-34.2354458468949,-2.90269141784383,
310.401864172681));
#15431=CARTESIAN_POINT('Ctrl Pts',(-34.1434652635131,-2.91788008880247,
310.406900449174));
#15432=CARTESIAN_POINT('Ctrl Pts',(-34.0506921691141,-2.92870398407811,
310.411936725666));
#15433=CARTESIAN_POINT('Ctrl Pts',(-33.957575010992,-2.93509500852077,310.416973002158));
#15434=CARTESIAN_POINT('Ctrl Pts',(-33.8644917126544,-2.94148370902321,
310.422007447331));
#15435=CARTESIAN_POINT('Ctrl Pts',(-33.7710650419058,-2.94344271052497,
310.427041892505));
#15436=CARTESIAN_POINT('Ctrl Pts',(-33.6777486467697,-2.94095576807704,
310.432076337678));
#15437=CARTESIAN_POINT('Ctrl Pts',(-33.5844400789956,-2.93846903423339,
310.437110360563));
#15438=CARTESIAN_POINT('Ctrl Pts',(-33.4912422125369,-2.93153710992043,
310.442144383447));
#15439=CARTESIAN_POINT('Ctrl Pts',(-33.3986076241413,-2.92019586292178,
310.447178406332));
#15440=CARTESIAN_POINT('Ctrl Pts',(-33.3059548920983,-2.90885239459747,
310.452213415194));
#15441=CARTESIAN_POINT('Ctrl Pts',(-33.2138660981168,-2.89309794278401,
310.457248424055));
#15442=CARTESIAN_POINT('Ctrl Pts',(-33.1227864912185,-2.87301997346749,
310.462283432917));
#15443=CARTESIAN_POINT('Ctrl Pts',(-33.0316068060052,-2.85291994246881,
310.467323974248));
#15444=CARTESIAN_POINT('Ctrl Pts',(-32.941438955873,-2.82848700682606,310.47236451558));
#15445=CARTESIAN_POINT('Ctrl Pts',(-32.85271552034,-2.79985922017207,310.477405056911));
#15446=CARTESIAN_POINT('Ctrl Pts',(-32.763937574495,-2.77121384504694,310.482448695074));
#15447=CARTESIAN_POINT('Ctrl Pts',(-32.6766062254526,-2.73836864438079,
310.487492333236));
#15448=CARTESIAN_POINT('Ctrl Pts',(-32.5911344206962,-2.70150999097119,
310.492535971399));
#15449=CARTESIAN_POINT('Ctrl Pts',(-32.5055242183565,-2.66459165532409,
310.497587776317));
#15450=CARTESIAN_POINT('Ctrl Pts',(-32.4217799700218,-2.62364708804665,
310.502639581235));
#15451=CARTESIAN_POINT('Ctrl Pts',(-32.3402901977767,-2.57890869903316,
310.507691386153));
#15452=CARTESIAN_POINT('Ctrl Pts',(-32.2990404953244,-2.55626235723886,
310.510248583749));
#15453=CARTESIAN_POINT('Ctrl Pts',(-32.2583680087024,-2.53264460754716,
310.512805781346));
#15454=CARTESIAN_POINT('Ctrl Pts',(-32.2183200952352,-2.50808968060854,
310.515362978942));
#15455=CARTESIAN_POINT('Ctrl Pts',(-32.1391970933683,-2.45957630346107,
310.520415255894));
#15456=CARTESIAN_POINT('Ctrl Pts',(-32.0622300048175,-2.40722802069624,
310.525467532846));
#15457=CARTESIAN_POINT('Ctrl Pts',(-31.987814328418,-2.35126225806393,310.530519809798));
#15458=CARTESIAN_POINT('Ctrl Pts',(-31.9135012850222,-2.2953736825863,310.535565118725));
#15459=CARTESIAN_POINT('Ctrl Pts',(-31.8417330133074,-2.23587780607076,
310.540610427651));
#15460=CARTESIAN_POINT('Ctrl Pts',(-31.7728782193927,-2.17303662510217,
310.545655736577));
#15461=CARTESIAN_POINT('Ctrl Pts',(-31.7040971139568,-2.11026269683695,
310.550695646008));
#15462=CARTESIAN_POINT('Ctrl Pts',(-31.6382236151875,-2.04415087807505,
310.555735555439));
#15463=CARTESIAN_POINT('Ctrl Pts',(-31.5755944689269,-1.975004245763,310.56077546487));
#15464=CARTESIAN_POINT('Ctrl Pts',(-31.513010467863,-1.90590745667101,310.565811741365));
#15465=CARTESIAN_POINT('Ctrl Pts',(-31.4536664683148,-1.8337805305052,310.570848017859));
#15466=CARTESIAN_POINT('Ctrl Pts',(-31.397862588501,-1.75896357163216,310.575884294354));
#15467=CARTESIAN_POINT('Ctrl Pts',(-31.3420790004076,-1.68417381812222,
310.580918739529));
#15468=CARTESIAN_POINT('Ctrl Pts',(-31.2898332400781,-1.60669633088394,
310.585953184704));
#15469=CARTESIAN_POINT('Ctrl Pts',(-31.2413846548929,-1.52690366778402,
310.59098762988));
#15470=CARTESIAN_POINT('Ctrl Pts',(-31.192940133566,-1.44711769767798,310.596021652767));
#15471=CARTESIAN_POINT('Ctrl Pts',(-31.148292384532,-1.3650173176519,310.601055675654));
#15472=CARTESIAN_POINT('Ctrl Pts',(-31.1076563667832,-1.28100240874095,
310.606089698541));
#15473=CARTESIAN_POINT('Ctrl Pts',(-31.06701238996,-1.19697104445505,310.611124707405));
#15474=CARTESIAN_POINT('Ctrl Pts',(-31.030381898013,-1.11102480663302,310.616159716268));
#15475=CARTESIAN_POINT('Ctrl Pts',(-30.9979325056523,-1.02358536137399,
310.621194725132));
#15476=CARTESIAN_POINT('Ctrl Pts',(-30.9654474578841,-0.936049837611584,
310.626235266466));
#15477=CARTESIAN_POINT('Ctrl Pts',(-30.937152835064,-0.847018248452105,
310.6312758078));
#15478=CARTESIAN_POINT('Ctrl Pts',(-30.9131668640838,-0.756929007225038,
310.636316349133));
#15479=CARTESIAN_POINT('Ctrl Pts',(-30.8891661564926,-0.666784416556086,
310.641359987298));
#15480=CARTESIAN_POINT('Ctrl Pts',(-30.8694794644035,-0.575581314118212,
310.646403625463));
#15481=CARTESIAN_POINT('Ctrl Pts',(-30.8541737630365,-0.483767778881916,
310.651447263627));
#15482=CARTESIAN_POINT('Ctrl Pts',(-30.8388432783848,-0.39180557741157,
310.656499068548));
#15483=CARTESIAN_POINT('Ctrl Pts',(-30.827907998374,-0.299231410511365,
310.661550873468));
#15484=CARTESIAN_POINT('Ctrl Pts',(-30.8213829689193,-0.206497757341061,
310.666602678388));
#15485=CARTESIAN_POINT('Ctrl Pts',(-30.81808003269,-0.159556460775926,310.669159875962));
#15486=CARTESIAN_POINT('Ctrl Pts',(-30.8159063177971,-0.112574291881349,
310.671717073537));
#15487=CARTESIAN_POINT('Ctrl Pts',(-30.814858696737,-0.0656096002259395,
310.674274271111));
#15488=CARTESIAN_POINT('Ctrl Pts',(-30.81278890292,0.0271789395537369,310.679326548055));
#15489=CARTESIAN_POINT('Ctrl Pts',(-30.815110515912,0.120232072311605,310.684378825));
#15490=CARTESIAN_POINT('Ctrl Pts',(-30.8218549564799,0.213099569194949,
310.689431101944));
#15491=CARTESIAN_POINT('Ctrl Pts',(-30.8285900952148,0.305838984595543,
310.694476410863));
#15492=CARTESIAN_POINT('Ctrl Pts',(-30.8397359083539,0.398392833634469,
310.699521719781));
#15493=CARTESIAN_POINT('Ctrl Pts',(-30.8552718378466,0.490309271450782,
310.7045670287));
#15494=CARTESIAN_POINT('Ctrl Pts',(-30.8707911407698,0.582127340190802,
310.709606938123));
#15495=CARTESIAN_POINT('Ctrl Pts',(-30.8906911478108,0.673308917910803,
310.714646847546));
#15496=CARTESIAN_POINT('Ctrl Pts',(-30.9148994576439,0.763406778219993,
310.719686756969));
#15497=CARTESIAN_POINT('Ctrl Pts',(-30.9390903173126,0.853439692959391,
310.724723033456));
#15498=CARTESIAN_POINT('Ctrl Pts',(-30.9675831920734,0.942390015186752,
310.729759309943));
#15499=CARTESIAN_POINT('Ctrl Pts',(-31.0002547166145,1.02982125558468,310.73479558643));
#15500=CARTESIAN_POINT('Ctrl Pts',(-31.0329143609523,1.11722070374403,310.739830031598));
#15501=CARTESIAN_POINT('Ctrl Pts',(-31.0697494811424,1.20310175169881,310.744864476765));
#15502=CARTESIAN_POINT('Ctrl Pts',(-31.1105873489966,1.28704460735787,310.749898921933));
#15503=CARTESIAN_POINT('Ctrl Pts',(-31.1514217913783,1.37098042190631,310.754932944812));
#15504=CARTESIAN_POINT('Ctrl Pts',(-31.1962581193606,1.45297796798695,310.759966967692));
#15505=CARTESIAN_POINT('Ctrl Pts',(-31.2448765954274,1.53263997033799,310.765000990571));
#15506=CARTESIAN_POINT('Ctrl Pts',(-31.2935045940337,1.61231757549331,310.770035999427));
#15507=CARTESIAN_POINT('Ctrl Pts',(-31.3459159801803,1.68965834943481,310.775071008283));
#15508=CARTESIAN_POINT('Ctrl Pts',(-31.4018470617087,1.76429301796272,310.780106017139));
#15509=CARTESIAN_POINT('Ctrl Pts',(-31.457839600337,1.83900969510125,310.785146558466));
#15510=CARTESIAN_POINT('Ctrl Pts',(-31.5173592873925,1.9110139753696,310.790187099792));
#15511=CARTESIAN_POINT('Ctrl Pts',(-31.5801016043343,1.97996903195367,310.795227641118));
#15512=CARTESIAN_POINT('Ctrl Pts',(-31.6428824691898,2.04896645346304,310.800271279276));
#15513=CARTESIAN_POINT('Ctrl Pts',(-31.7088895915387,2.11491060796936,310.805314917433));
#15514=CARTESIAN_POINT('Ctrl Pts',(-31.7777825701013,2.17750251819656,310.81035855559));
#15515=CARTESIAN_POINT('Ctrl Pts',(-31.8467871014961,2.24019577844526,310.815410360503));
#15516=CARTESIAN_POINT('Ctrl Pts',(-31.9186864756149,2.29952567564314,310.820462165416));
#15517=CARTESIAN_POINT('Ctrl Pts',(-31.9931084678045,2.35523450341486,310.825513970329));
#15518=CARTESIAN_POINT('Ctrl Pts',(-32.0307804972763,2.38343402535606,310.828071167979));
#15519=CARTESIAN_POINT('Ctrl Pts',(-32.0690984606701,2.41070641144219,310.83062836563));
#15520=CARTESIAN_POINT('Ctrl Pts',(-32.1080116130096,2.43702268924819,310.83318556328));
#15521=CARTESIAN_POINT('Ctrl Pts',(-32.184892656084,2.4890159811284,310.838237840233));
#15522=CARTESIAN_POINT('Ctrl Pts',(-32.2643744688606,2.53746096915058,310.843290117185));
#15523=CARTESIAN_POINT('Ctrl Pts',(-32.3460955868427,2.58208740027939,310.848342394138));
#15524=CARTESIAN_POINT('Ctrl Pts',(-32.4277039962628,2.62665228329182,310.853387703064));
#15525=CARTESIAN_POINT('Ctrl Pts',(-32.5115451872888,2.66740886353547,310.858433011991));
#15526=CARTESIAN_POINT('Ctrl Pts',(-32.5972281857368,2.7041297083826,310.863478320917));
#15527=CARTESIAN_POINT('Ctrl Pts',(-32.6828194861414,2.74081125453939,310.868518230348));
#15528=CARTESIAN_POINT('Ctrl Pts',(-32.7702482699579,2.77346547600095,310.873558139779));
#15529=CARTESIAN_POINT('Ctrl Pts',(-32.8590993676928,2.80191102313471,310.87859804921));
#15530=CARTESIAN_POINT('Ctrl Pts',(-32.9478864185641,2.83033606576011,310.883634325705));
#15531=CARTESIAN_POINT('Ctrl Pts',(-33.0380933236371,2.8545583290018,310.8886706022));
#15532=CARTESIAN_POINT('Ctrl Pts',(-33.129286337883,2.87444512082797,310.893706878694));
#15533=CARTESIAN_POINT('Ctrl Pts',(-33.2204461920115,2.89432468130691,310.89874132387));
#15534=CARTESIAN_POINT('Ctrl Pts',(-33.3125910093486,2.90987180767159,310.903775769045));
#15535=CARTESIAN_POINT('Ctrl Pts',(-33.4052743468349,2.92100434748797,310.908810214221));
#15536=CARTESIAN_POINT('Ctrl Pts',(-33.4979499100589,2.93213595350883,310.913844237108));
#15537=CARTESIAN_POINT('Ctrl Pts',(-33.5911634625136,2.93885365641506,310.918878259995));
#15538=CARTESIAN_POINT('Ctrl Pts',(-33.6844620299747,2.94112701671504,310.923912282882));
#15539=CARTESIAN_POINT('Ctrl Pts',(-33.7777788711309,2.94340082228116,310.928947291745));
#15540=CARTESIAN_POINT('Ctrl Pts',(-33.8711803162558,2.94122854601305,310.933982300609));
#15541=CARTESIAN_POINT('Ctrl Pts',(-33.9642131246277,2.93463186366688,310.939017309472));
#15542=CARTESIAN_POINT('Ctrl Pts',(-34.0573481574917,2.92802793288315,310.944057850806));
#15543=CARTESIAN_POINT('Ctrl Pts',(-34.1501133012287,2.91698992328308,310.94909839214));
#15544=CARTESIAN_POINT('Ctrl Pts',(-34.2420604806244,2.90159140420482,310.954138933473));
#15545=CARTESIAN_POINT('Ctrl Pts',(-34.3340641509496,2.88618342451382,310.959182571638));
#15546=CARTESIAN_POINT('Ctrl Pts',(-34.4252484226218,2.86640969600237,310.964226209802));
#15547=CARTESIAN_POINT('Ctrl Pts',(-34.5151776046413,2.84239445150339,310.969269847967));
#15548=CARTESIAN_POINT('Ctrl Pts',(-34.6052524017129,2.81834032106104,310.974321652887));
#15549=CARTESIAN_POINT('Ctrl Pts',(-34.6940676292192,2.79003109837152,310.979373457807));
#15550=CARTESIAN_POINT('Ctrl Pts',(-34.7812050550307,2.75764012026162,310.984425262726));
#15551=CARTESIAN_POINT('Ctrl Pts',(-34.8253135701994,2.74124397433485,310.986982460301));
#15552=CARTESIAN_POINT('Ctrl Pts',(-34.868992526545,2.72380270133821,310.989539657876));
#15553=CARTESIAN_POINT('Ctrl Pts',(-34.9121900856443,2.70534326849836,310.99209685545));
#15554=CARTESIAN_POINT('Ctrl Pts',(-34.9975358700768,2.66887281024228,310.997149132419));
#15555=CARTESIAN_POINT('Ctrl Pts',(-35.0813073487881,2.62829430803813,311.002201409388));
#15556=CARTESIAN_POINT('Ctrl Pts',(-35.1630815699805,2.58376525812304,311.007253686357));
#15557=CARTESIAN_POINT('Ctrl Pts',(-35.2447430093745,2.53929762201609,311.0122989953));
#15558=CARTESIAN_POINT('Ctrl Pts',(-35.3244122781905,2.4908904757454,311.017344304243));
#15559=CARTESIAN_POINT('Ctrl Pts',(-35.4016864391525,2.43874931375529,311.022389613186));
#15560=CARTESIAN_POINT('Ctrl Pts',(-35.4788779012206,2.3866639532953,311.027429522634));
#15561=CARTESIAN_POINT('Ctrl Pts',(-35.5536789839904,2.33085276721458,311.032469432082));
#15562=CARTESIAN_POINT('Ctrl Pts',(-35.6257123855913,2.27156654765511,311.037509341529));
#15563=CARTESIAN_POINT('Ctrl Pts',(-35.6976938630922,2.21232306359795,311.042545618041));
#15564=CARTESIAN_POINT('Ctrl Pts',(-35.7669112828091,2.14960980644723,311.047581894552));
#15565=CARTESIAN_POINT('Ctrl Pts',(-35.8330181862139,2.08371953620005,311.052618171064));
#15566=CARTESIAN_POINT('Ctrl Pts',(-35.899101051455,2.01785322534312,311.057652616256));
#15567=CARTESIAN_POINT('Ctrl Pts',(-35.9620753330269,1.948812509708,311.062687061448));
#15568=CARTESIAN_POINT('Ctrl Pts',(-36.0216301810279,1.87692819553516,311.06772150664));
#15569=CARTESIAN_POINT('Ctrl Pts',(-36.081180033579,1.8050499110056,311.072755529544));
#15570=CARTESIAN_POINT('Ctrl Pts',(-36.1373107395428,1.73032884439181,311.077789552448));
#15571=CARTESIAN_POINT('Ctrl Pts',(-36.1897513839202,1.65312929951775,311.082823575352));
#15572=CARTESIAN_POINT('Ctrl Pts',(-36.2422022994558,1.57591463414406,311.087858584233));
#15573=CARTESIAN_POINT('Ctrl Pts',(-36.2909614687216,1.49622089409765,311.092893593113));
#15574=CARTESIAN_POINT('Ctrl Pts',(-36.3358016426966,1.41444083232241,311.097928601994));
#15575=CARTESIAN_POINT('Ctrl Pts',(-36.3806910870742,1.33257091057981,311.102969143344));
#15576=CARTESIAN_POINT('Ctrl Pts',(-36.4216527265697,1.24861048125042,311.108009684694));
#15577=CARTESIAN_POINT('Ctrl Pts',(-36.4585057337172,1.16297605997046,311.113050226045));
#15578=CARTESIAN_POINT('Ctrl Pts',(-36.4953813827839,1.07728902622267,311.118093864226));
#15579=CARTESIAN_POINT('Ctrl Pts',(-36.5281432182783,0.989926368693434,
311.123137502407));
#15580=CARTESIAN_POINT('Ctrl Pts',(-36.5566597098044,0.901321631153508,
311.128181140589));
#15581=CARTESIAN_POINT('Ctrl Pts',(-36.5852223757779,0.812573423131264,
311.133232945525));
#15582=CARTESIAN_POINT('Ctrl Pts',(-36.6095258587224,0.722579548340074,
311.138284750462));
#15583=CARTESIAN_POINT('Ctrl Pts',(-36.6294893627108,0.631785468102651,
311.143336555398));
#15584=CARTESIAN_POINT('Ctrl Pts',(-36.6395947846885,0.585825976501504,
311.145893752805));
#15585=CARTESIAN_POINT('Ctrl Pts',(-36.648588983502,0.539661560233308,311.148450950212));
#15586=CARTESIAN_POINT('Ctrl Pts',(-36.6564665537928,0.49335040206328,311.151008147619));
#15587=CARTESIAN_POINT('Ctrl Pts',(-36.6809714621854,0.349289397639362,
311.158962870444));
#15588=CARTESIAN_POINT('Ctrl Pts',(-36.6947476817154,0.203354132616775,
311.16691759327));
#15589=CARTESIAN_POINT('Ctrl Pts',(-36.6975782807065,0.0568199948794944,
311.174872316094));
#15590=CARTESIAN_POINT('Ctrl Pts',(-36.6979283747003,0.038696367452575,
311.1758561717));
#15591=CARTESIAN_POINT('Ctrl Pts',(-36.6981110795063,0.0205636243529551,
311.176840027305));
#15592=CARTESIAN_POINT('Ctrl Pts',(-36.6981260264713,0.00242422312990352,
311.17782388291));
#15593=CARTESIAN_POINT('',(-36.6981269603261,0.000618107681218697,312.177823882879));
#15594=CARTESIAN_POINT('Ctrl Pts',(-36.6981260264717,0.00242422262950888,
311.177823882937));
#15595=CARTESIAN_POINT('Ctrl Pts',(-36.6982015303164,-0.08920607281627,
311.182793781264));
#15596=CARTESIAN_POINT('Ctrl Pts',(-36.6939920174391,-0.180989576697442,
311.18776367959));
#15597=CARTESIAN_POINT('Ctrl Pts',(-36.6854811606969,-0.272485502704996,
311.192733577917));
#15598=CARTESIAN_POINT('Ctrl Pts',(-36.6769797232138,-0.363880167012936,
311.197697975885));
#15599=CARTESIAN_POINT('Ctrl Pts',(-36.6641864429127,-0.454987431746313,
311.202662373854));
#15600=CARTESIAN_POINT('Ctrl Pts',(-36.6471370372109,-0.54536695058065,
311.207626771822));
#15601=CARTESIAN_POINT('Ctrl Pts',(-36.6300979046698,-0.635692011017376,
311.212588178481));
#15602=CARTESIAN_POINT('Ctrl Pts',(-36.6088078208921,-0.725289746294086,
311.217549585139));
#15603=CARTESIAN_POINT('Ctrl Pts',(-36.5833541612158,-0.813726441564893,
311.222510991797));
#15604=CARTESIAN_POINT('Ctrl Pts',(-36.5579082237446,-0.902136306654335,
311.22747089325));
#15605=CARTESIAN_POINT('Ctrl Pts',(-36.5283013451067,-0.989385390561597,
311.232430794703));
#15606=CARTESIAN_POINT('Ctrl Pts',(-36.4946713648304,-1.07505297552896,
311.237390696155));
#15607=CARTESIAN_POINT('Ctrl Pts',(-36.461041526873,-1.1607201979592,311.242350576618));
#15608=CARTESIAN_POINT('Ctrl Pts',(-36.4233887902628,-1.24480550829142,
311.24731045708));
#15609=CARTESIAN_POINT('Ctrl Pts',(-36.3818994618245,-1.32690734844808,
311.252270337543));
#15610=CARTESIAN_POINT('Ctrl Pts',(-36.3403707750732,-1.40908707344996,
311.257234923132));
#15611=CARTESIAN_POINT('Ctrl Pts',(-36.2949984353924,-1.48927916026966,
311.262199508721));
#15612=CARTESIAN_POINT('Ctrl Pts',(-36.2460149194563,-1.56710633791168,
311.26716409431));
#15613=CARTESIAN_POINT('Ctrl Pts',(-36.1970083707436,-1.64497011104825,
311.27213101432));
#15614=CARTESIAN_POINT('Ctrl Pts',(-36.1443875290459,-1.72046638555712,
311.277097934331));
#15615=CARTESIAN_POINT('Ctrl Pts',(-36.0884270842775,-1.79324857024776,
311.282064854342));
#15616=CARTESIAN_POINT('Ctrl Pts',(-36.0323714334215,-1.86615458002741,
311.287040224625));
#15617=CARTESIAN_POINT('Ctrl Pts',(-35.9729651288959,-1.9363369277628,311.292015594909));
#15618=CARTESIAN_POINT('Ctrl Pts',(-35.9105217632539,-2.00348379401826,
311.296990965192));
#15619=CARTESIAN_POINT('Ctrl Pts',(-35.8564355063254,-2.06164405848986,
311.301300456725));
#15620=CARTESIAN_POINT('Ctrl Pts',(-35.8000714528542,-2.11752745102219,
311.305609948257));
#15621=CARTESIAN_POINT('Ctrl Pts',(-35.7416530584122,-2.17095609620858,
311.309919439789));
#15622=CARTESIAN_POINT('Ctrl Pts',(-35.6731656491964,-2.23359372125257,
311.314971716779));
#15623=CARTESIAN_POINT('Ctrl Pts',(-35.601588345643,-2.29309973061535,311.32002399377));
#15624=CARTESIAN_POINT('Ctrl Pts',(-35.5272393903716,-2.34915410097772,
311.32507627076));
#15625=CARTESIAN_POINT('Ctrl Pts',(-35.452992976089,-2.40513116197449,311.330121579725));
#15626=CARTESIAN_POINT('Ctrl Pts',(-35.3759828577769,-2.4576657784631,311.335166888689));
#15627=CARTESIAN_POINT('Ctrl Pts',(-35.2965627104359,-2.50647599227066,
311.340212197653));
#15628=CARTESIAN_POINT('Ctrl Pts',(-35.2172275586343,-2.55523396932734,
311.345252107122));
#15629=CARTESIAN_POINT('Ctrl Pts',(-35.1354878808409,-2.60027523483785,
311.35029201659));
#15630=CARTESIAN_POINT('Ctrl Pts',(-35.0517280019881,-2.64135989768432,
311.355331926058));
#15631=CARTESIAN_POINT('Ctrl Pts',(-34.9680285000898,-2.6824149453158,311.36036820259));
#15632=CARTESIAN_POINT('Ctrl Pts',(-34.8823120893024,-2.71951886405753,
311.365404479121));
#15633=CARTESIAN_POINT('Ctrl Pts',(-34.7949885596874,-2.75247719559713,
311.370440755652));
#15634=CARTESIAN_POINT('Ctrl Pts',(-34.7076967831545,-2.78542354263936,
311.375475200863));
#15635=CARTESIAN_POINT('Ctrl Pts',(-34.6187994639651,-2.81422714045836,
311.380509646075));
#15636=CARTESIAN_POINT('Ctrl Pts',(-34.5287263166366,-2.83874168161893,
311.385544091286));
#15637=CARTESIAN_POINT('Ctrl Pts',(-34.438660724638,-2.86325416650133,311.390578114208));
#15638=CARTESIAN_POINT('Ctrl Pts',(-34.3474199293088,-2.88347819353403,
311.395612137131));
#15639=CARTESIAN_POINT('Ctrl Pts',(-34.2554476394487,-2.89931766528675,
311.400646160053));
#15640=CARTESIAN_POINT('Ctrl Pts',(-34.1634573356725,-2.9151602393969,311.405681168952));
#15641=CARTESIAN_POINT('Ctrl Pts',(-34.070735690674,-2.92661647767692,311.41071617785));
#15642=CARTESIAN_POINT('Ctrl Pts',(-33.9777342682891,-2.93364180326024,
311.415751186749));
#15643=CARTESIAN_POINT('Ctrl Pts',(-33.8846306559204,-2.94067484827288,
311.420791728116));
#15644=CARTESIAN_POINT('Ctrl Pts',(-33.7912470961995,-2.94326722859512,
311.425832269483));
#15645=CARTESIAN_POINT('Ctrl Pts',(-33.6980376016428,-2.94142645987693,
311.430872810851));
#15646=CARTESIAN_POINT('Ctrl Pts',(-33.6047708406207,-2.93958456021902,
311.435916449048));
#15647=CARTESIAN_POINT('Ctrl Pts',(-33.5116788005859,-2.9333041191332,311.440960087246));
#15648=CARTESIAN_POINT('Ctrl Pts',(-33.419210621842,-2.92264457933385,311.446003725443));
#15649=CARTESIAN_POINT('Ctrl Pts',(-33.3265927168774,-2.9119677794064,311.451055530395));
#15650=CARTESIAN_POINT('Ctrl Pts',(-33.2346011277437,-2.89689779674547,
311.456107335347));
#15651=CARTESIAN_POINT('Ctrl Pts',(-33.1436748748383,-2.87754519746376,
311.461159140299));
#15652=CARTESIAN_POINT('Ctrl Pts',(-33.0976484816358,-2.86774901302232,
311.463716337518));
#15653=CARTESIAN_POINT('Ctrl Pts',(-33.0518948267786,-2.85685627741267,
311.466273534738));
#15654=CARTESIAN_POINT('Ctrl Pts',(-33.006469123943,-2.84488611916128,311.468830731957));
#15655=CARTESIAN_POINT('Ctrl Pts',(-32.9167211621574,-2.82123657191711,
311.47388300906));
#15656=CARTESIAN_POINT('Ctrl Pts',(-32.8279323153016,-2.79329347552532,
311.478935286163));
#15657=CARTESIAN_POINT('Ctrl Pts',(-32.7405439656881,-2.76115103699805,
311.483987563266));
#15658=CARTESIAN_POINT('Ctrl Pts',(-32.6532761407779,-2.72905292884073,
311.489032872344));
#15659=CARTESIAN_POINT('Ctrl Pts',(-32.5674053882141,-2.69276713935733,
311.494078181422));
#15660=CARTESIAN_POINT('Ctrl Pts',(-32.483360280933,-2.65243827723499,311.4991234905));
#15661=CARTESIAN_POINT('Ctrl Pts',(-32.3994051188064,-2.61215257509963,
311.504163400083));
#15662=CARTESIAN_POINT('Ctrl Pts',(-32.3172721168548,-2.56783259185325,
311.509203309667));
#15663=CARTESIAN_POINT('Ctrl Pts',(-32.2373710843367,-2.51967148491972,
311.51424321925));
#15664=CARTESIAN_POINT('Ctrl Pts',(-32.1575276471636,-2.47154509412792,
311.519279495898));
#15665=CARTESIAN_POINT('Ctrl Pts',(-32.0799133609419,-2.41958331172726,
311.524315772545));
#15666=CARTESIAN_POINT('Ctrl Pts',(-32.0049136338218,-2.36402530816736,
311.529352049192));
#15667=CARTESIAN_POINT('Ctrl Pts',(-31.9299411785199,-2.30848750691804,
311.534386494521));
#15668=CARTESIAN_POINT('Ctrl Pts',(-31.857581750232,-2.2493563465259,311.53942093985));
#15669=CARTESIAN_POINT('Ctrl Pts',(-31.7881910703001,-2.18691382481923,
311.544455385178));
#15670=CARTESIAN_POINT('Ctrl Pts',(-31.7188062108451,-2.12447654077925,
311.549489408218));
#15671=CARTESIAN_POINT('Ctrl Pts',(-31.6523899347525,-2.05872874497333,
311.554523431259));
#15672=CARTESIAN_POINT('Ctrl Pts',(-31.5892633338439,-1.98999139265296,
311.559557454299));
#15673=CARTESIAN_POINT('Ctrl Pts',(-31.5261243688003,-1.92124057726179,
311.564592463315));
#15674=CARTESIAN_POINT('Ctrl Pts',(-31.4662766587785,-1.8494993699054,311.569627472332));
#15675=CARTESIAN_POINT('Ctrl Pts',(-31.4100022394138,-1.77512323213051,
311.574662481349));
#15676=CARTESIAN_POINT('Ctrl Pts',(-31.3536659857059,-1.70066536984051,
311.579703022834));
#15677=CARTESIAN_POINT('Ctrl Pts',(-31.3009111285474,-1.62356715267035,
311.58474356432));
#15678=CARTESIAN_POINT('Ctrl Pts',(-31.2519772385529,-1.54421431341205,
311.589784105805));
#15679=CARTESIAN_POINT('Ctrl Pts',(-31.2030132843353,-1.46481272100019,
311.594827744121));
#15680=CARTESIAN_POINT('Ctrl Pts',(-31.1578751855412,-1.38315413735048,
311.599871382437));
#15681=CARTESIAN_POINT('Ctrl Pts',(-31.1167562219282,-1.29964832263674,
311.604915020754));
#15682=CARTESIAN_POINT('Ctrl Pts',(-31.0755706777221,-1.21600729374959,
311.609966825823));
#15683=CARTESIAN_POINT('Ctrl Pts',(-31.0384174376808,-1.13051346942785,
311.615018630892));
#15684=CARTESIAN_POINT('Ctrl Pts',(-31.005441324204,-1.04359579053353,311.620070435962));
#15685=CARTESIAN_POINT('Ctrl Pts',(-30.9887489961861,-0.99959853756195,
311.622627632017));
#15686=CARTESIAN_POINT('Ctrl Pts',(-30.9731261874234,-0.955236679455002,
311.625184828072));
#15687=CARTESIAN_POINT('Ctrl Pts',(-30.958586720807,-0.910566990931599,
311.627742024127));
#15688=CARTESIAN_POINT('Ctrl Pts',(-30.9298609591932,-0.822312665120583,
311.632794300543));
#15689=CARTESIAN_POINT('Ctrl Pts',(-30.9052639847033,-0.732539269766924,
311.637846576958));
#15690=CARTESIAN_POINT('Ctrl Pts',(-30.8849556511083,-0.641668871198852,
311.642898853374));
#15691=CARTESIAN_POINT('Ctrl Pts',(-30.8646753264713,-0.550923799761345,
311.647944161764));
#15692=CARTESIAN_POINT('Ctrl Pts',(-30.8486719852641,-0.459085161372459,
311.652989470153));
#15693=CARTESIAN_POINT('Ctrl Pts',(-30.8370561740245,-0.366591551295231,
311.658034778543));
#15694=CARTESIAN_POINT('Ctrl Pts',(-30.8254527940393,-0.2741969279853,311.663074687437));
#15695=CARTESIAN_POINT('Ctrl Pts',(-30.8182276659885,-0.181149164659398,
311.668114596332));
#15696=CARTESIAN_POINT('Ctrl Pts',(-30.8154403620448,-0.0878973765402973,
311.673154505227));
#15697=CARTESIAN_POINT('Ctrl Pts',(-30.8126550672823,0.00528719259989155,
311.678190781188));
#15698=CARTESIAN_POINT('Ctrl Pts',(-30.8143012515402,0.098675051434181,
311.68322705715));
#15699=CARTESIAN_POINT('Ctrl Pts',(-30.8203865910775,0.191812677162036,
311.688263333111));
#15700=CARTESIAN_POINT('Ctrl Pts',(-30.8264697178317,0.284916435697699,
311.693297777755));
#15701=CARTESIAN_POINT('Ctrl Pts',(-30.8369887641721,0.377769699025832,
311.6983322224));
#15702=CARTESIAN_POINT('Ctrl Pts',(-30.8518993257529,0.469920705470309,
311.703366667044));
#15703=CARTESIAN_POINT('Ctrl Pts',(-30.8668086366464,0.562063982353962,
311.708400689403));
#15704=CARTESIAN_POINT('Ctrl Pts',(-30.8861086592593,0.653504680946815,
311.713434711761));
#15705=CARTESIAN_POINT('Ctrl Pts',(-30.9097034849681,0.743799051683824,
311.71846873412));
#15706=CARTESIAN_POINT('Ctrl Pts',(-30.9333029320361,0.834111107769477,
311.723503742459));
#15707=CARTESIAN_POINT('Ctrl Pts',(-30.9611987401457,0.923275960390066,
311.728538750797));
#15708=CARTESIAN_POINT('Ctrl Pts',(-30.9932448407682,1.0108640040238,311.733573759136));
#15709=CARTESIAN_POINT('Ctrl Pts',(-31.0253261537173,1.09854828959467,311.738614299953));
#15710=CARTESIAN_POINT('Ctrl Pts',(-31.061566709298,1.18465188984667,311.74365484077));
#15711=CARTESIAN_POINT('Ctrl Pts',(-31.10177199305,1.26876450257491,311.748695381587));
#15712=CARTESIAN_POINT('Ctrl Pts',(-31.1420019783427,1.35292879286734,311.753739019239));
#15713=CARTESIAN_POINT('Ctrl Pts',(-31.1862013308537,1.43509926946008,311.758782656891));
#15714=CARTESIAN_POINT('Ctrl Pts',(-31.2341302670182,1.51489153124244,311.763826294542));
#15715=CARTESIAN_POINT('Ctrl Pts',(-31.2821368107472,1.59481299437146,311.768878098961));
#15716=CARTESIAN_POINT('Ctrl Pts',(-31.3338847479845,1.67234818587392,311.773929903379));
#15717=CARTESIAN_POINT('Ctrl Pts',(-31.3890919270446,1.74714305190724,311.778981707798));
#15718=CARTESIAN_POINT('Ctrl Pts',(-31.417037576359,1.7850039086341,311.781538910631));
#15719=CARTESIAN_POINT('Ctrl Pts',(-31.4458689738935,1.82216314442311,311.784096113463));
#15720=CARTESIAN_POINT('Ctrl Pts',(-31.4755458783913,1.85857839021061,311.786653316296));
#15721=CARTESIAN_POINT('Ctrl Pts',(-31.534178676157,1.9305241600941,311.791705593785));
#15722=CARTESIAN_POINT('Ctrl Pts',(-31.5963245793649,1.99982180600417,311.796757871274));
#15723=CARTESIAN_POINT('Ctrl Pts',(-31.6617153560105,2.06610836107927,311.801810148764));
#15724=CARTESIAN_POINT('Ctrl Pts',(-31.7270159466201,2.13230349467329,311.806855458223));
#15725=CARTESIAN_POINT('Ctrl Pts',(-31.7955522084267,2.19549547615848,311.811900767682));
#15726=CARTESIAN_POINT('Ctrl Pts',(-31.8670153102018,2.25535383654962,311.816946077142));
#15727=CARTESIAN_POINT('Ctrl Pts',(-31.9384019320278,2.31514813640814,311.821985987101));
#15728=CARTESIAN_POINT('Ctrl Pts',(-32.0127088291449,2.37161562267808,311.827025897061));
#15729=CARTESIAN_POINT('Ctrl Pts',(-32.0895907196,2.42446298011023,311.83206580702));
#15730=CARTESIAN_POINT('Ctrl Pts',(-32.1664171908701,2.47727224329867,311.837102084034));
#15731=CARTESIAN_POINT('Ctrl Pts',(-32.2458146010754,2.52646631349717,311.842138361048));
#15732=CARTESIAN_POINT('Ctrl Pts',(-32.327405856766,2.57179311428893,311.847174638063));
#15733=CARTESIAN_POINT('Ctrl Pts',(-32.4089674436963,2.61710343304501,311.852209083752));
#15734=CARTESIAN_POINT('Ctrl Pts',(-32.4927209033532,2.65854906051797,311.857243529441));
#15735=CARTESIAN_POINT('Ctrl Pts',(-32.5782624164361,2.69592265528625,311.862277975131));
#15736=CARTESIAN_POINT('Ctrl Pts',(-32.6637967542063,2.73329311511788,311.867311998525));
#15737=CARTESIAN_POINT('Ctrl Pts',(-32.7511184400287,2.76659204366298,311.87234602192));
#15738=CARTESIAN_POINT('Ctrl Pts',(-32.8398024957292,2.79565973548009,311.877380045315));
#15739=CARTESIAN_POINT('Ctrl Pts',(-32.9285039211922,2.82473312052919,311.882415054679));
#15740=CARTESIAN_POINT('Ctrl Pts',(-33.018567824221,2.84957348497027,311.887450064043));
#15741=CARTESIAN_POINT('Ctrl Pts',(-33.1095539506286,2.87007095019703,311.892485073408));
#15742=CARTESIAN_POINT('Ctrl Pts',(-33.2006400523817,2.89059093799119,311.897525615229));
#15743=CARTESIAN_POINT('Ctrl Pts',(-33.2926499661888,2.90675840337116,311.90256615705));
#15744=CARTESIAN_POINT('Ctrl Pts',(-33.3851334272274,2.91851464793662,311.907606698871));
#15745=CARTESIAN_POINT('Ctrl Pts',(-33.4776737085474,2.9302781153408,311.912650337516));
#15746=CARTESIAN_POINT('Ctrl Pts',(-33.5706876737533,2.93762493153835,311.917693976161));
#15747=CARTESIAN_POINT('Ctrl Pts',(-33.6637223142929,2.94054848104763,311.922737614806));
#15748=CARTESIAN_POINT('Ctrl Pts',(-33.7569075980058,2.94347676441489,311.927789420191));
#15749=CARTESIAN_POINT('Ctrl Pts',(-33.8501131802449,2.94196748977706,311.932841225576));
#15750=CARTESIAN_POINT('Ctrl Pts',(-33.9428886175165,2.93606609388428,311.937893030961));
#15751=CARTESIAN_POINT('Ctrl Pts',(-33.9898509674947,2.93307884394587,311.940450223463));
#15752=CARTESIAN_POINT('Ctrl Pts',(-34.0367032179707,2.92896701435596,311.943007415965));
#15753=CARTESIAN_POINT('Ctrl Pts',(-34.0833879581403,2.92374148682963,311.945564608466));
#15754=CARTESIAN_POINT('Ctrl Pts',(-34.1756235996956,2.9134173448915,311.950616886579));
#15755=CARTESIAN_POINT('Ctrl Pts',(-34.2675357765239,2.89870573751808,311.955669164692));
#15756=CARTESIAN_POINT('Ctrl Pts',(-34.3586740912813,2.87963557298944,311.960721442804));
#15757=CARTESIAN_POINT('Ctrl Pts',(-34.4496867096227,2.86059170970787,311.965766752901));
#15758=CARTESIAN_POINT('Ctrl Pts',(-34.5399271556838,2.83720132458121,311.970812062998));
#15759=CARTESIAN_POINT('Ctrl Pts',(-34.6289503631172,2.80954505585649,311.975857373094));
#15760=CARTESIAN_POINT('Ctrl Pts',(-34.7178782979768,2.78191838485106,311.980897283704));
#15761=CARTESIAN_POINT('Ctrl Pts',(-34.805591161522,2.7500350356528,311.985937194313));
#15762=CARTESIAN_POINT('Ctrl Pts',(-34.8916553791004,2.71402641063402,311.990977104922));
#15763=CARTESIAN_POINT('Ctrl Pts',(-34.9776575588258,2.67804374178903,311.996013382602));
#15764=CARTESIAN_POINT('Ctrl Pts',(-35.0620130460367,2.63794187860835,312.001049660282));
#15765=CARTESIAN_POINT('Ctrl Pts',(-35.1443057044382,2.59390130010153,312.006085937962));
#15766=CARTESIAN_POINT('Ctrl Pts',(-35.2265684391902,2.54987673584024,312.011120384326));
#15767=CARTESIAN_POINT('Ctrl Pts',(-35.3067694439806,2.50191651090943,312.01615483069));
#15768=CARTESIAN_POINT('Ctrl Pts',(-35.3845157142294,2.45024779922945,312.021189277055));
#15769=CARTESIAN_POINT('Ctrl Pts',(-35.4622554631727,2.39858342148666,312.026223301133));
#15770=CARTESIAN_POINT('Ctrl Pts',(-35.5375405170566,2.34321142151244,312.031257325212));
#15771=CARTESIAN_POINT('Ctrl Pts',(-35.6100064567246,2.28440255944164,312.03629134929));
#15772=CARTESIAN_POINT('Ctrl Pts',(-35.6824865897655,2.22558217890967,312.041326359346));
#15773=CARTESIAN_POINT('Ctrl Pts',(-35.7521461672983,2.16332387961225,312.046361369402));
#15774=CARTESIAN_POINT('Ctrl Pts',(-35.8186543834119,2.09793824905908,312.051396379458));
#15775=CARTESIAN_POINT('Ctrl Pts',(-35.8852356786866,2.03248077284068,312.056436921978));
#15776=CARTESIAN_POINT('Ctrl Pts',(-35.9486583832679,1.96388941802114,312.061477464498));
#15777=CARTESIAN_POINT('Ctrl Pts',(-36.0086292938647,1.89251090615609,312.066518007017));
#15778=CARTESIAN_POINT('Ctrl Pts',(-36.0686370496362,1.82108854046741,312.071561646366));
#15779=CARTESIAN_POINT('Ctrl Pts',(-36.1251885204058,1.74687596180443,312.076605285716));
#15780=CARTESIAN_POINT('Ctrl Pts',(-36.1780328000423,1.67025040579686,312.081648925065));
#15781=CARTESIAN_POINT('Ctrl Pts',(-36.2309626459783,1.59350077646818,312.086700731155));
#15782=CARTESIAN_POINT('Ctrl Pts',(-36.2801730828093,1.51433074652193,312.091752537245));
#15783=CARTESIAN_POINT('Ctrl Pts',(-36.3254583509524,1.43314358624782,312.096804343336));
#15784=CARTESIAN_POINT('Ctrl Pts',(-36.3483814087769,1.39204726406881,312.099361529102));
#15785=CARTESIAN_POINT('Ctrl Pts',(-36.3702994732512,1.35043443810575,312.101918714868));
#15786=CARTESIAN_POINT('Ctrl Pts',(-36.3911905990756,1.30835926332855,312.104475900635));
#15787=CARTESIAN_POINT('Ctrl Pts',(-36.4354099813449,1.21930048051519,312.109888590018));
#15788=CARTESIAN_POINT('Ctrl Pts',(-36.4751667113802,1.12788489735598,312.1153012794));
#15789=CARTESIAN_POINT('Ctrl Pts',(-36.5102214562109,1.03456651085936,312.120713968783));
#15790=CARTESIAN_POINT('Ctrl Pts',(-36.5451612253897,0.94155419825884,312.126108905148));
#15791=CARTESIAN_POINT('Ctrl Pts',(-36.5754296261192,0.846651844587571,
312.131503841514));
#15792=CARTESIAN_POINT('Ctrl Pts',(-36.6008348302367,0.750334261706711,
312.136898777879));
#15793=CARTESIAN_POINT('Ctrl Pts',(-36.6261882476559,0.654213015355424,
312.142282717051));
#15794=CARTESIAN_POINT('Ctrl Pts',(-36.6466981192475,0.556682616613729,
312.147666656223));
#15795=CARTESIAN_POINT('Ctrl Pts',(-36.6622213344253,0.458235601217396,
312.153050595395));
#15796=CARTESIAN_POINT('Ctrl Pts',(-36.6776995355044,0.360074061710941,
312.158418922262));
#15797=CARTESIAN_POINT('Ctrl Pts',(-36.688219842539,0.261001543111834,312.163787249129));
#15798=CARTESIAN_POINT('Ctrl Pts',(-36.6936897286263,0.16152202257669,312.169155575996));
#15799=CARTESIAN_POINT('Ctrl Pts',(-36.69663382725,0.107978399396601,312.172045011624));
#15800=CARTESIAN_POINT('Ctrl Pts',(-36.6981156782847,0.0543171084516736,
312.174934447252));
#15801=CARTESIAN_POINT('Ctrl Pts',(-36.6981269603261,0.000618107681204032,
312.177823882879));
#15802=CARTESIAN_POINT('',(-36.6981257736749,-0.00271372645954632,313.177823882956));
#15803=CARTESIAN_POINT('Ctrl Pts',(-36.6981269603262,0.000618107113904726,
312.17782388291));
#15804=CARTESIAN_POINT('Ctrl Pts',(-36.6981472510316,-0.0959594160750109,
312.183020525908));
#15805=CARTESIAN_POINT('Ctrl Pts',(-36.693407656044,-0.192478386360223,
312.188217168906));
#15806=CARTESIAN_POINT('Ctrl Pts',(-36.683951507351,-0.288457626098284,
312.193413811904));
#15807=CARTESIAN_POINT('Ctrl Pts',(-36.6744864103721,-0.384527690305954,
312.198615372448));
#15808=CARTESIAN_POINT('Ctrl Pts',(-36.6602959088366,-0.48005660696899,
312.203816932992));
#15809=CARTESIAN_POINT('Ctrl Pts',(-36.6414748179091,-0.574571244878503,
312.209018493536));
#15810=CARTESIAN_POINT('Ctrl Pts',(-36.6226162191874,-0.669274237203749,
312.214230420061));
#15811=CARTESIAN_POINT('Ctrl Pts',(-36.5991086761896,-0.762958518130133,
312.219442346586));
#15812=CARTESIAN_POINT('Ctrl Pts',(-36.5710976252041,-0.855163447205775,
312.22465427311));
#15813=CARTESIAN_POINT('Ctrl Pts',(-36.5430558604506,-0.947469477836219,
312.229871914448));
#15814=CARTESIAN_POINT('Ctrl Pts',(-36.5105008799693,-1.03829254542981,
312.235089555785));
#15815=CARTESIAN_POINT('Ctrl Pts',(-36.473626493746,-1.12719148274162,312.240307197122));
#15816=CARTESIAN_POINT('Ctrl Pts',(-36.4366733133957,-1.21628038156532,
312.245535987648));
#15817=CARTESIAN_POINT('Ctrl Pts',(-36.3953824581606,-1.30343657214762,
312.250764778174));
#15818=CARTESIAN_POINT('Ctrl Pts',(-36.34999418024,-1.38824247964953,312.2559935687));
#15819=CARTESIAN_POINT('Ctrl Pts',(-36.3286008411863,-1.42821494866716,
312.258458110068));
#15820=CARTESIAN_POINT('Ctrl Pts',(-36.3062978410755,-1.46766568669913,
312.260922651436));
#15821=CARTESIAN_POINT('Ctrl Pts',(-36.2831135879918,-1.50655332191096,
312.263387192804));
#15822=CARTESIAN_POINT('Ctrl Pts',(-36.2355861173756,-1.58627255777278,
312.268439476224));
#15823=CARTESIAN_POINT('Ctrl Pts',(-36.1841972653882,-1.66388364616725,
312.273491759643));
#15824=CARTESIAN_POINT('Ctrl Pts',(-36.1291595320973,-1.73898841901895,
312.278544043063));
#15825=CARTESIAN_POINT('Ctrl Pts',(-36.0741977062961,-1.81398960812129,
312.283589358424));
#15826=CARTESIAN_POINT('Ctrl Pts',(-36.0155972597245,-1.88649099532476,
312.288634673786));
#15827=CARTESIAN_POINT('Ctrl Pts',(-35.95361559243,-1.95612064994633,312.293679989147));
#15828=CARTESIAN_POINT('Ctrl Pts',(-35.8917002584041,-2.02567578636307,
312.298719904972));
#15829=CARTESIAN_POINT('Ctrl Pts',(-35.8264111899827,-2.09236496889872,
312.303759820796));
#15830=CARTESIAN_POINT('Ctrl Pts',(-35.7580472611431,-2.15584771474055,
312.308799736621));
#15831=CARTESIAN_POINT('Ctrl Pts',(-35.6897326124361,-2.21928469905018,
312.313836019423));
#15832=CARTESIAN_POINT('Ctrl Pts',(-35.618347833547,-2.27951953938701,312.318872302225));
#15833=CARTESIAN_POINT('Ctrl Pts',(-35.5442292776944,-2.33624791810079,
312.323908585027));
#15834=CARTESIAN_POINT('Ctrl Pts',(-35.4701376740366,-2.39295566831891,
312.328943036454));
#15835=CARTESIAN_POINT('Ctrl Pts',(-35.39331462073,-2.44615922024994,312.333977487881));
#15836=CARTESIAN_POINT('Ctrl Pts',(-35.3141294281189,-2.49559462106297,
312.339011939308));
#15837=CARTESIAN_POINT('Ctrl Pts',(-35.2349508785342,-2.54502587462749,
312.344045968383));
#15838=CARTESIAN_POINT('Ctrl Pts',(-35.153410960587,-2.5906893704818,312.349079997459));
#15839=CARTESIAN_POINT('Ctrl Pts',(-35.0699068567329,-2.63236520156467,
312.354114026534));
#15840=CARTESIAN_POINT('Ctrl Pts',(-34.9863863987443,-2.67404919478714,
312.359149041515));
#15841=CARTESIAN_POINT('Ctrl Pts',(-34.9009013885088,-2.71174377417091,
312.364184056497));
#15842=CARTESIAN_POINT('Ctrl Pts',(-34.8138713796262,-2.74527610283581,
312.369219071478));
#15843=CARTESIAN_POINT('Ctrl Pts',(-34.7267457447288,-2.7788452758375,312.374259618785));
#15844=CARTESIAN_POINT('Ctrl Pts',(-34.6380721377659,-2.80824290918259,
312.379300166093));
#15845=CARTESIAN_POINT('Ctrl Pts',(-34.5482874714049,-2.83334534209292,
312.384340713401));
#15846=CARTESIAN_POINT('Ctrl Pts',(-34.4584476440895,-2.85846319717071,
312.389384357467));
#15847=CARTESIAN_POINT('Ctrl Pts',(-34.3674958311872,-2.87928049935423,
312.394428001532));
#15848=CARTESIAN_POINT('Ctrl Pts',(-34.2758792465645,-2.89572471558444,
312.399471645598));
#15849=CARTESIAN_POINT('Ctrl Pts',(-34.1841143178764,-2.91219555801879,
312.404523456249));
#15850=CARTESIAN_POINT('Ctrl Pts',(-34.0916829085481,-2.92427912097878,
312.409575266901));
#15851=CARTESIAN_POINT('Ctrl Pts',(-33.9990372770051,-2.93195474207839,
312.414627077552));
#15852=CARTESIAN_POINT('Ctrl Pts',(-33.9521417224921,-2.93584000360344,
312.417184213359));
#15853=CARTESIAN_POINT('Ctrl Pts',(-33.9051912835796,-2.9385966924718,312.419741349166));
#15854=CARTESIAN_POINT('Ctrl Pts',(-33.8582443398703,-2.94022721129784,
312.422298484973));
#15855=CARTESIAN_POINT('Ctrl Pts',(-33.7654884768215,-2.94344872411588,
312.427350769956));
#15856=CARTESIAN_POINT('Ctrl Pts',(-33.6724135305641,-2.94228243713677,
312.43240305494));
#15857=CARTESIAN_POINT('Ctrl Pts',(-33.5794693066669,-2.93669134409157,
312.437455339923));
#15858=CARTESIAN_POINT('Ctrl Pts',(-33.4866532680901,-2.93110796208018,
312.442500656977));
#15859=CARTESIAN_POINT('Ctrl Pts',(-33.3939680332237,-2.92111192695525,
312.447545974032));
#15860=CARTESIAN_POINT('Ctrl Pts',(-33.3018656686103,-2.90671818720992,
312.452591291086));
#15861=CARTESIAN_POINT('Ctrl Pts',(-33.2098618703539,-2.89233985139583,
312.457631208729));
#15862=CARTESIAN_POINT('Ctrl Pts',(-33.1184401390671,-2.87357323376419,
312.462671126372));
#15863=CARTESIAN_POINT('Ctrl Pts',(-33.0280485666081,-2.85048517941255,
312.467711044015));
#15864=CARTESIAN_POINT('Ctrl Pts',(-32.9377221497179,-2.82741376726849,
312.472747328812));
#15865=CARTESIAN_POINT('Ctrl Pts',(-32.8484248449244,-2.80002721943948,
312.477783613609));
#15866=CARTESIAN_POINT('Ctrl Pts',(-32.7605946403837,-2.76844347434933,
312.482819898405));
#15867=CARTESIAN_POINT('Ctrl Pts',(-32.6727963721871,-2.73687121356978,
312.487854351936));
#15868=CARTESIAN_POINT('Ctrl Pts',(-32.5864645620957,-2.70110493759086,
312.492888805466));
#15869=CARTESIAN_POINT('Ctrl Pts',(-32.5020211150125,-2.66131215115555,
312.497923258996));
#15870=CARTESIAN_POINT('Ctrl Pts',(-32.4175847503165,-2.62152270219566,
312.502957290279));
#15871=CARTESIAN_POINT('Ctrl Pts',(-32.3350368355249,-2.57770760376478,
312.507991321563));
#15872=CARTESIAN_POINT('Ctrl Pts',(-32.2547773439412,-2.5300816457994,312.513025352847));
#15873=CARTESIAN_POINT('Ctrl Pts',(-32.1745021320575,-2.4824463594128,312.518060370138));
#15874=CARTESIAN_POINT('Ctrl Pts',(-32.0965166154096,-2.43099895809983,
312.523095387429));
#15875=CARTESIAN_POINT('Ctrl Pts',(-32.0211933139959,-2.3759985306241,312.528130404721));
#15876=CARTESIAN_POINT('Ctrl Pts',(-31.9457872475172,-2.32093766880901,
312.533170954477));
#15877=CARTESIAN_POINT('Ctrl Pts',(-31.8730495947316,-2.26231625025901,
312.538211504233));
#15878=CARTESIAN_POINT('Ctrl Pts',(-31.8033209375348,-2.20043458974651,
312.54325205399));
#15879=CARTESIAN_POINT('Ctrl Pts',(-31.7335494400637,-2.13851491004045,
312.548295700587));
#15880=CARTESIAN_POINT('Ctrl Pts',(-31.6667909361748,-2.07333131083482,
312.553339347184));
#15881=CARTESIAN_POINT('Ctrl Pts',(-31.6033486065793,-2.00522045672617,
312.558382993781));
#15882=CARTESIAN_POINT('Ctrl Pts',(-31.5398035509794,-1.93699931732458,
312.563434807065));
#15883=CARTESIAN_POINT('Ctrl Pts',(-31.4795856759634,-1.86584179924721,
312.568486620349));
#15884=CARTESIAN_POINT('Ctrl Pts',(-31.4229572895715,-1.79211690033832,
312.573538433634));
#15885=CARTESIAN_POINT('Ctrl Pts',(-31.3942932713292,-1.75479901116856,
312.576095548137));
#15886=CARTESIAN_POINT('Ctrl Pts',(-31.3665482396374,-1.71682377199302,
312.57865266264));
#15887=CARTESIAN_POINT('Ctrl Pts',(-31.3397517917505,-1.67824155916049,
312.581209777143));
#15888=CARTESIAN_POINT('Ctrl Pts',(-31.2868086003306,-1.60201259448517,
312.586262006573));
#15889=CARTESIAN_POINT('Ctrl Pts',(-31.2373810767036,-1.52313904501004,
312.591314236002));
#15890=CARTESIAN_POINT('Ctrl Pts',(-31.1917439396311,-1.44197898394981,
312.596366465432));
#15891=CARTESIAN_POINT('Ctrl Pts',(-31.1461697458949,-1.360930859907,312.601411726761));
#15892=CARTESIAN_POINT('Ctrl Pts',(-31.1043757663751,-1.27760287473358,
312.60645698809));
#15893=CARTESIAN_POINT('Ctrl Pts',(-31.0665942694062,-1.19238314110958,
312.611502249418));
#15894=CARTESIAN_POINT('Ctrl Pts',(-31.0288532066941,-1.10725461076966,
312.616542111242));
#15895=CARTESIAN_POINT('Ctrl Pts',(-30.9951162702355,-1.02023876008219,
312.621581973065));
#15896=CARTESIAN_POINT('Ctrl Pts',(-30.9655699495079,-0.931748467658128,
312.626621834889));
#15897=CARTESIAN_POINT('Ctrl Pts',(-30.9360449258947,-0.843321959415589,
312.631658063958));
#15898=CARTESIAN_POINT('Ctrl Pts',(-30.9107046544222,-0.7534235420511,312.636694293028));
#15899=CARTESIAN_POINT('Ctrl Pts',(-30.8896872014526,-0.662485272670189,
312.641730522097));
#15900=CARTESIAN_POINT('Ctrl Pts',(-30.8686773904944,-0.57158006872722,
312.646764919978));
#15901=CARTESIAN_POINT('Ctrl Pts',(-30.8519873754526,-0.479636196309396,
312.651799317859));
#15902=CARTESIAN_POINT('Ctrl Pts',(-30.8397048446733,-0.387099037193126,
312.65683371574));
#15903=CARTESIAN_POINT('Ctrl Pts',(-30.8274233437007,-0.294569636688765,
312.661867691521));
#15904=CARTESIAN_POINT('Ctrl Pts',(-30.8195486505376,-0.201447488814254,
312.666901667302));
#15905=CARTESIAN_POINT('Ctrl Pts',(-30.8161168256602,-0.108185148072898,
312.671935643083));
#15906=CARTESIAN_POINT('Ctrl Pts',(-30.8126843284428,-0.0149045359998572,
312.676970605087));
#15907=CARTESIAN_POINT('Ctrl Pts',(-30.8136964441276,0.0785158795345645,
312.68200556709));
#15908=CARTESIAN_POINT('Ctrl Pts',(-30.8191371252647,0.171622630616089,
312.687040529094));
#15909=CARTESIAN_POINT('Ctrl Pts',(-30.8245837853907,0.264831700547405,
312.692081024225));
#15910=CARTESIAN_POINT('Ctrl Pts',(-30.8344686995876,0.357725973770652,
312.697121519356));
#15911=CARTESIAN_POINT('Ctrl Pts',(-30.8487238666971,0.449856503334521,
312.702162014487));
#15912=CARTESIAN_POINT('Ctrl Pts',(-30.862987792904,0.542043642567136,312.707205606754));
#15913=CARTESIAN_POINT('Ctrl Pts',(-30.8816272292481,0.633465668903467,
312.712249199021));
#15914=CARTESIAN_POINT('Ctrl Pts',(-30.9045233612998,0.7236853900019,312.717292791288));
#15915=CARTESIAN_POINT('Ctrl Pts',(-30.9274565717259,0.814051214407146,
312.722344551231));
#15916=CARTESIAN_POINT('Ctrl Pts',(-30.9546601101224,0.90321042216864,312.727396311175));
#15917=CARTESIAN_POINT('Ctrl Pts',(-30.9859658451968,0.990742669154766,
312.732448071118));
#15918=CARTESIAN_POINT('Ctrl Pts',(-31.0018156910173,1.03505955281071,312.735005737183));
#15919=CARTESIAN_POINT('Ctrl Pts',(-31.0187163010574,1.0789597352799,312.737563403247));
#15920=CARTESIAN_POINT('Ctrl Pts',(-31.0366413382941,1.12239101849619,312.740121069312));
#15921=CARTESIAN_POINT('Ctrl Pts',(-31.0720500112955,1.20818409580586,312.745173419281));
#15922=CARTESIAN_POINT('Ctrl Pts',(-31.1115860558145,1.2924539236927,312.75022576925));
#15923=CARTESIAN_POINT('Ctrl Pts',(-31.1550972300989,1.37477561976373,312.755278119219));
#15924=CARTESIAN_POINT('Ctrl Pts',(-31.198548393021,1.45698377633121,312.7603235009));
#15925=CARTESIAN_POINT('Ctrl Pts',(-31.2459635853537,1.53724875094398,312.765368882581));
#15926=CARTESIAN_POINT('Ctrl Pts',(-31.2971423226019,1.61516507890224,312.770414264261));
#15927=CARTESIAN_POINT('Ctrl Pts',(-31.3482662854831,1.69299801641815,312.775454246091));
#15928=CARTESIAN_POINT('Ctrl Pts',(-31.403145544521,1.7684869342367,312.78049422792));
#15929=CARTESIAN_POINT('Ctrl Pts',(-31.4615340029829,1.84125143913817,312.785534209749));
#15930=CARTESIAN_POINT('Ctrl Pts',(-31.5198803641481,1.91396348180589,312.790570557819));
#15931=CARTESIAN_POINT('Ctrl Pts',(-31.5817306186015,1.98395467032566,312.795606905888));
#15932=CARTESIAN_POINT('Ctrl Pts',(-31.6467963223114,2.05087493173238,312.800643253958));
#15933=CARTESIAN_POINT('Ctrl Pts',(-31.7118383598756,2.11777085244102,312.805677770173));
#15934=CARTESIAN_POINT('Ctrl Pts',(-31.7800932138977,2.18159774684734,312.810712286387));
#15935=CARTESIAN_POINT('Ctrl Pts',(-31.8512339550428,2.24204067560063,312.815746802602));
#15936=CARTESIAN_POINT('Ctrl Pts',(-31.9223687202328,2.30247852703496,312.820780895907));
#15937=CARTESIAN_POINT('Ctrl Pts',(-31.9963885518909,2.35953269049083,312.825814989213));
#15938=CARTESIAN_POINT('Ctrl Pts',(-32.0729325298441,2.41292774251732,312.830849082519));
#15939=CARTESIAN_POINT('Ctrl Pts',(-32.1494914889608,2.46633324500677,312.835884161096));
#15940=CARTESIAN_POINT('Ctrl Pts',(-32.2285752109656,2.51607795992609,312.840919239673));
#15941=CARTESIAN_POINT('Ctrl Pts',(-32.3097937864364,2.56192977309703,312.84595431825));
#15942=CARTESIAN_POINT('Ctrl Pts',(-32.3911015796948,2.60783195402318,312.85099492781));
#15943=CARTESIAN_POINT('Ctrl Pts',(-32.4745485200974,2.64983247843533,312.85603553737));
#15944=CARTESIAN_POINT('Ctrl Pts',(-32.5597203608117,2.68774535498985,312.86107614693));
#15945=CARTESIAN_POINT('Ctrl Pts',(-32.6449445165234,2.72568151872499,312.866119852578));
#15946=CARTESIAN_POINT('Ctrl Pts',(-32.7318952680904,2.75952487516603,312.871163558226));
#15947=CARTESIAN_POINT('Ctrl Pts',(-32.8201407292169,2.78913851459979,312.876207263873));
#15948=CARTESIAN_POINT('Ctrl Pts',(-32.908529045529,2.8188000937452,312.881259134468));
#15949=CARTESIAN_POINT('Ctrl Pts',(-32.9982158287868,2.84421816524307,312.886311005062));
#15950=CARTESIAN_POINT('Ctrl Pts',(-33.0887566456159,2.86530640183156,312.891362875657));
#15951=CARTESIAN_POINT('Ctrl Pts',(-33.1345747571572,2.87597808792916,312.893919370932));
#15952=CARTESIAN_POINT('Ctrl Pts',(-33.1806114499131,2.88554178628865,312.896475866207));
#15953=CARTESIAN_POINT('Ctrl Pts',(-33.2268086614984,2.89399137348184,312.899032361481));
#15954=CARTESIAN_POINT('Ctrl Pts',(-33.318106787295,2.91069003229739,312.90408468432));
#15955=CARTESIAN_POINT('Ctrl Pts',(-33.4103597300015,2.92309408354272,312.909137007159));
#15956=CARTESIAN_POINT('Ctrl Pts',(-33.5031278634048,2.93110140119747,312.914189329998));
#15957=CARTESIAN_POINT('Ctrl Pts',(-33.595768070785,2.9390976768676,312.919234685751));
#15958=CARTESIAN_POINT('Ctrl Pts',(-33.6889216183641,2.94270922910701,312.924280041504));
#15959=CARTESIAN_POINT('Ctrl Pts',(-33.7821390761671,2.9418850033962,312.929325397257));
#15960=CARTESIAN_POINT('Ctrl Pts',(-33.8752567894102,2.94106165962354,312.934365354378));
#15961=CARTESIAN_POINT('Ctrl Pts',(-33.9684378351084,2.93581197594322,312.939405311499));
#15962=CARTESIAN_POINT('Ctrl Pts',(-34.0612291570517,2.92613681996839,312.944445268619));
#15963=CARTESIAN_POINT('Ctrl Pts',(-34.1539536122272,2.9164686360508,312.949481593874));
#15964=CARTESIAN_POINT('Ctrl Pts',(-34.2462884612768,2.90238136447852,312.954517919128));
#15965=CARTESIAN_POINT('Ctrl Pts',(-34.3377832022272,2.88392789296007,312.959554244383));
#15966=CARTESIAN_POINT('Ctrl Pts',(-34.429244685366,2.86548112917226,312.964588738962));
#15967=CARTESIAN_POINT('Ctrl Pts',(-34.5198662320261,2.84267140610266,312.969623233542));
#15968=CARTESIAN_POINT('Ctrl Pts',(-34.609206032639,2.81560299175241,312.974657728121));
#15969=CARTESIAN_POINT('Ctrl Pts',(-34.6985383497843,2.78853684476344,312.979691800991));
#15970=CARTESIAN_POINT('Ctrl Pts',(-34.7865887092408,2.75721284473957,312.98472587386));
#15971=CARTESIAN_POINT('Ctrl Pts',(-34.8729301119596,2.72178523501266,312.98975994673));
#15972=CARTESIAN_POINT('Ctrl Pts',(-34.9592884343651,2.68635068279884,312.994795006089));
#15973=CARTESIAN_POINT('Ctrl Pts',(-35.0439367241078,2.64681109279851,312.999830065449));
#15974=CARTESIAN_POINT('Ctrl Pts',(-35.1264686903429,2.60336853344491,313.004865124808));
#15975=CARTESIAN_POINT('Ctrl Pts',(-35.2090913493738,2.55987823589556,313.009905717098));
#15976=CARTESIAN_POINT('Ctrl Pts',(-35.2895926490284,2.5124766150874,313.014946309388));
#15977=CARTESIAN_POINT('Ctrl Pts',(-35.3675918910899,2.46141117779781,313.019986901678));
#15978=CARTESIAN_POINT('Ctrl Pts',(-35.4456390594115,2.41031436359532,313.025030591135));
#15979=CARTESIAN_POINT('Ctrl Pts',(-35.5211807501152,2.35554951173853,313.030074280593));
#15980=CARTESIAN_POINT('Ctrl Pts',(-35.5938679726108,2.29740553895508,313.03511797005));
#15981=CARTESIAN_POINT('Ctrl Pts',(-35.6666728906397,2.23916741914481,313.040169826276));
#15982=CARTESIAN_POINT('Ctrl Pts',(-35.7366137803689,2.17753954857637,313.045221682502));
#15983=CARTESIAN_POINT('Ctrl Pts',(-35.8033773782909,2.11284878588248,313.050273538729));
#15984=CARTESIAN_POINT('Ctrl Pts',(-35.8371659136847,2.08010929620596,313.052830243703));
#15985=CARTESIAN_POINT('Ctrl Pts',(-35.8701412748032,2.04658585996007,313.055386948677));
#15986=CARTESIAN_POINT('Ctrl Pts',(-35.9022668598925,2.01232398241272,313.057943653651));
#15987=CARTESIAN_POINT('Ctrl Pts',(-35.96503030191,1.94538688667172,313.062938663203));
#15988=CARTESIAN_POINT('Ctrl Pts',(-36.0247853386703,1.87537575228471,313.067933672756));
#15989=CARTESIAN_POINT('Ctrl Pts',(-36.0812105112672,1.80259556836398,313.072928682308));
#15990=CARTESIAN_POINT('Ctrl Pts',(-36.1375118641317,1.72997509370923,313.077912730782));
#15991=CARTESIAN_POINT('Ctrl Pts',(-36.1904976205588,1.65459802241339,313.082896779256));
#15992=CARTESIAN_POINT('Ctrl Pts',(-36.2398843068163,1.57680492335112,313.08788082773));
#15993=CARTESIAN_POINT('Ctrl Pts',(-36.289223520604,1.49908660214551,313.092860085336));
#15994=CARTESIAN_POINT('Ctrl Pts',(-36.3349702892972,1.41895724594861,313.097839342942));
#15995=CARTESIAN_POINT('Ctrl Pts',(-36.3768824674861,1.33678903048679,313.102818600548));
#15996=CARTESIAN_POINT('Ctrl Pts',(-36.4187667597575,1.25467548496026,313.107794545247));
#15997=CARTESIAN_POINT('Ctrl Pts',(-36.4568213220447,1.17052617915665,313.112770489945));
#15998=CARTESIAN_POINT('Ctrl Pts',(-36.4908489574481,1.08473957869907,313.117746434644));
#15999=CARTESIAN_POINT('Ctrl Pts',(-36.5250852286384,0.998426989448164,
313.122752888666));
#16000=CARTESIAN_POINT('Ctrl Pts',(-36.5552447983262,0.91045736888119,313.127759342688));
#16001=CARTESIAN_POINT('Ctrl Pts',(-36.5811755664054,0.821258022888564,
313.13276579671));
#16002=CARTESIAN_POINT('Ctrl Pts',(-36.6069440501183,0.73261691949377,313.137740918486));
#16003=CARTESIAN_POINT('Ctrl Pts',(-36.6285364213618,0.642761892145859,
313.142716040262));
#16004=CARTESIAN_POINT('Ctrl Pts',(-36.6458536373614,0.552126894200304,
313.147691162037));
#16005=CARTESIAN_POINT('Ctrl Pts',(-36.6633344435117,0.460635696679663,
313.152713282183));
#16006=CARTESIAN_POINT('Ctrl Pts',(-36.6764587920037,0.368350176472159,
313.157735402328));
#16007=CARTESIAN_POINT('Ctrl Pts',(-36.6851780352602,0.275724828049647,
313.162757522474));
#16008=CARTESIAN_POINT('Ctrl Pts',(-36.6938972785166,0.183099479627143,
313.167779642619));
#16009=CARTESIAN_POINT('Ctrl Pts',(-36.6982114179565,0.0901347795703585,
313.172801762765));
#16010=CARTESIAN_POINT('Ctrl Pts',(-36.6981257736756,-0.00271372561674938,
313.17782388291));
#16011=CARTESIAN_POINT('',(-35.0450520381518,2.64462403965778,313.999935411543));
#16012=CARTESIAN_POINT('Ctrl Pts',(-36.6981257736749,-0.00271372645954639,
313.177823882956));
#16013=CARTESIAN_POINT('Ctrl Pts',(-36.698013371732,-0.124570656500899,
313.184415051462));
#16014=CARTESIAN_POINT('Ctrl Pts',(-36.6903263421818,-0.246089772706434,
313.191006219968));
#16015=CARTESIAN_POINT('Ctrl Pts',(-36.67521211245,-0.366478176336686,313.197597388474));
#16016=CARTESIAN_POINT('Ctrl Pts',(-36.6604922568569,-0.483725296961528,
313.204016574256));
#16017=CARTESIAN_POINT('Ctrl Pts',(-36.6387280713999,-0.599900445757358,
313.210435760038));
#16018=CARTESIAN_POINT('Ctrl Pts',(-36.610097867168,-0.714292960573622,
313.21685494582));
#16019=CARTESIAN_POINT('Ctrl Pts',(-36.5875606888686,-0.804340676673007,
313.221908012621));
#16020=CARTESIAN_POINT('Ctrl Pts',(-36.5607171932186,-0.893482126933944,
313.226961079422));
#16021=CARTESIAN_POINT('Ctrl Pts',(-36.5296561804346,-0.981274694152054,
313.232014146222));
#16022=CARTESIAN_POINT('Ctrl Pts',(-36.4986380120204,-1.06894616366983,
313.237060243017));
#16023=CARTESIAN_POINT('Ctrl Pts',(-36.4634140334802,-1.15527203236899,
313.242106339811));
#16024=CARTESIAN_POINT('Ctrl Pts',(-36.4241236001709,-1.23982187279091,
313.247152436605));
#16025=CARTESIAN_POINT('Ctrl Pts',(-36.384875232422,-1.32428119152297,313.252193130891));
#16026=CARTESIAN_POINT('Ctrl Pts',(-36.3415692497026,-1.40696786088303,
313.257233825177));
#16027=CARTESIAN_POINT('Ctrl Pts',(-36.2943937834563,-1.48746961791609,
313.262274519463));
#16028=CARTESIAN_POINT('Ctrl Pts',(-36.2472523894463,-1.5679132329718,313.267311573134));
#16029=CARTESIAN_POINT('Ctrl Pts',(-36.1962472907678,-1.64617469026335,
313.272348626805));
#16030=CARTESIAN_POINT('Ctrl Pts',(-36.1416129292153,-1.7218655586366,313.277385680475));
#16031=CARTESIAN_POINT('Ctrl Pts',(-36.0869984857682,-1.79752883231216,
313.282420897782));
#16032=CARTESIAN_POINT('Ctrl Pts',(-36.0287576676608,-1.87062301912678,
313.287456115089));
#16033=CARTESIAN_POINT('Ctrl Pts',(-35.9671681084419,-1.94078884180407,
313.292491332396));
#16034=CARTESIAN_POINT('Ctrl Pts',(-35.9055837875718,-2.0109486966996,313.297526121445));
#16035=CARTESIAN_POINT('Ctrl Pts',(-35.8406515849871,-2.07818034901596,
313.302560910493));
#16036=CARTESIAN_POINT('Ctrl Pts',(-35.7726885189259,-2.14215866411762,
313.307595699542));
#16037=CARTESIAN_POINT('Ctrl Pts',(-35.7047122366137,-2.20614942058663,
313.312631467668));
#16038=CARTESIAN_POINT('Ctrl Pts',(-35.6337042438977,-2.26688527927062,
313.317667235793));
#16039=CARTESIAN_POINT('Ctrl Pts',(-35.5600165494819,-2.32407972849336,
313.322703003918));
#16040=CARTESIAN_POINT('Ctrl Pts',(-35.4862481190206,-2.38133684290998,
313.327744289491));
#16041=CARTESIAN_POINT('Ctrl Pts',(-35.4097944775704,-2.43504452987422,
313.332785575064));
#16042=CARTESIAN_POINT('Ctrl Pts',(-35.3310384321946,-2.4849583618845,313.337826860637));
#16043=CARTESIAN_POINT('Ctrl Pts',(-35.252234123565,-2.53490278207288,313.342871235609));
#16044=CARTESIAN_POINT('Ctrl Pts',(-35.1711249877506,-2.58104849926232,
313.347915610581));
#16045=CARTESIAN_POINT('Ctrl Pts',(-35.0881184382244,-2.62319707147263,
313.352959985553));
#16046=CARTESIAN_POINT('Ctrl Pts',(-35.0049778100673,-2.66541372533304,
313.358012508592));
#16047=CARTESIAN_POINT('Ctrl Pts',(-34.9199340541806,-2.7036201627846,313.36306503163));
#16048=CARTESIAN_POINT('Ctrl Pts',(-34.8334143707933,-2.73766615480207,
313.368117554669));
#16049=CARTESIAN_POINT('Ctrl Pts',(-34.7897555456756,-2.75484615307824,
313.370667115776));
#16050=CARTESIAN_POINT('Ctrl Pts',(-34.7457211432041,-2.77096755745217,
313.373216676883));
#16051=CARTESIAN_POINT('Ctrl Pts',(-34.7013672446505,-2.78601595968905,
313.375766237989));
#16052=CARTESIAN_POINT('Ctrl Pts',(-34.6134720100465,-2.81583707774537,
313.380818652297));
#16053=CARTESIAN_POINT('Ctrl Pts',(-34.5240066289806,-2.84154809311651,
313.385871066604));
#16054=CARTESIAN_POINT('Ctrl Pts',(-34.4333912087129,-2.86298397232829,
313.390923480911));
#16055=CARTESIAN_POINT('Ctrl Pts',(-34.3429006011634,-2.88439032598752,
313.395968936076));
#16056=CARTESIAN_POINT('Ctrl Pts',(-34.2512635306771,-2.90153314339791,
313.401014391241));
#16057=CARTESIAN_POINT('Ctrl Pts',(-34.1589172359201,-2.91429649249943,
313.406059846406));
#16058=CARTESIAN_POINT('Ctrl Pts',(-34.0666696108495,-2.92704620428439,
313.41109991063));
#16059=CARTESIAN_POINT('Ctrl Pts',(-33.9737147054072,-2.93542568821401,
313.416139974853));
#16060=CARTESIAN_POINT('Ctrl Pts',(-33.8805009020536,-2.93936985402837,
313.421180039077));
#16061=CARTESIAN_POINT('Ctrl Pts',(-33.7873540677987,-2.94331118617195,
313.426216482286));
#16062=CARTESIAN_POINT('Ctrl Pts',(-33.6939491478886,-2.94282351513798,
313.431252925495));
#16063=CARTESIAN_POINT('Ctrl Pts',(-33.600739569472,-2.9378935887102,313.436289368704));
#16064=CARTESIAN_POINT('Ctrl Pts',(-33.5075637480035,-2.93296544771341,
313.441323987905));
#16065=CARTESIAN_POINT('Ctrl Pts',(-33.4145835706385,-2.92359827085021,
313.446358607107));
#16066=CARTESIAN_POINT('Ctrl Pts',(-33.3222513426158,-2.90983090436748,
313.451393226308));
#16067=CARTESIAN_POINT('Ctrl Pts',(-33.2299267299149,-2.89606467338131,
313.456427430267));
#16068=CARTESIAN_POINT('Ctrl Pts',(-33.1382503996357,-2.87789904003722,
313.461461634227));
#16069=CARTESIAN_POINT('Ctrl Pts',(-33.0476672780537,-2.85542444946311,
313.466495838186));
#16070=CARTESIAN_POINT('Ctrl Pts',(-32.9570662931595,-2.83294542682022,
313.471531034908));
#16071=CARTESIAN_POINT('Ctrl Pts',(-32.8675593761473,-2.80615586666568,
313.47656623163));
#16072=CARTESIAN_POINT('Ctrl Pts',(-32.7795779268821,-2.77519654411396,
313.481601428352));
#16073=CARTESIAN_POINT('Ctrl Pts',(-32.6914996494938,-2.74420314923082,
313.486642166568));
#16074=CARTESIAN_POINT('Ctrl Pts',(-32.6049506107236,-2.70903097937245,
313.491682904784));
#16075=CARTESIAN_POINT('Ctrl Pts',(-32.5203435052314,-2.66986948962524,
313.496723643));
#16076=CARTESIAN_POINT('Ctrl Pts',(-32.4356843295594,-2.63068389852384,
313.501767483462));
#16077=CARTESIAN_POINT('Ctrl Pts',(-32.3529698599341,-2.58750430519844,
313.506811323925));
#16078=CARTESIAN_POINT('Ctrl Pts',(-32.2725874490644,-2.54056574917254,
313.511855164388));
#16079=CARTESIAN_POINT('Ctrl Pts',(-32.1920747856778,-2.49355113340923,
313.516907177944));
#16080=CARTESIAN_POINT('Ctrl Pts',(-32.1139020971782,-2.4427656365906,313.5219591915));
#16081=CARTESIAN_POINT('Ctrl Pts',(-32.0384269135352,-2.38848703705688,
313.527011205056));
#16082=CARTESIAN_POINT('Ctrl Pts',(-32.0002495750241,-2.3610314898388,313.529566646757));
#16083=CARTESIAN_POINT('Ctrl Pts',(-31.9627618847262,-2.33268283049408,
313.532122088458));
#16084=CARTESIAN_POINT('Ctrl Pts',(-31.9260066147779,-2.30348068868517,
313.534677530159));
#16085=CARTESIAN_POINT('Ctrl Pts',(-31.8533945198067,-2.24579022151206,
313.539725948406));
#16086=CARTESIAN_POINT('Ctrl Pts',(-31.7833813566834,-2.18455843129818,
313.544774366654));
#16087=CARTESIAN_POINT('Ctrl Pts',(-31.7163331569566,-2.12004834257189,
313.549822784901));
#16088=CARTESIAN_POINT('Ctrl Pts',(-31.6493776542288,-2.05562744179774,
313.554864223495));
#16089=CARTESIAN_POINT('Ctrl Pts',(-31.5853792874978,-1.98793755438931,
313.559905662089));
#16090=CARTESIAN_POINT('Ctrl Pts',(-31.5246721392417,-1.91728273649867,
313.564947100682));
#16091=CARTESIAN_POINT('Ctrl Pts',(-31.4640300858115,-1.84670368008263,
313.569983133462));
#16092=CARTESIAN_POINT('Ctrl Pts',(-31.4066725249717,-1.77316634781203,
313.575019166241));
#16093=CARTESIAN_POINT('Ctrl Pts',(-31.3528968716914,-1.69701173507727,
313.580055199021));
#16094=CARTESIAN_POINT('Ctrl Pts',(-31.2991599408614,-1.62091195930001,
313.585087605484));
#16095=CARTESIAN_POINT('Ctrl Pts',(-31.2490000472261,-1.54219901129288,
313.590120011947));
#16096=CARTESIAN_POINT('Ctrl Pts',(-31.2026737868128,-1.46124623492275,
313.59515241841));
#16097=CARTESIAN_POINT('Ctrl Pts',(-31.1563643343673,-1.38032282961867,
313.600182999029));
#16098=CARTESIAN_POINT('Ctrl Pts',(-31.1138859729088,-1.29716159613364,
313.605213579648));
#16099=CARTESIAN_POINT('Ctrl Pts',(-31.0754509106536,-1.21216317737825,
313.610244160267));
#16100=CARTESIAN_POINT('Ctrl Pts',(-31.0370189971839,-1.1271717221027,313.615274328757));
#16101=CARTESIAN_POINT('Ctrl Pts',(-31.0026299075449,-1.04034378635827,
313.620304497246));
#16102=CARTESIAN_POINT('Ctrl Pts',(-30.9724484854758,-0.95210177352955,
313.625334665736));
#16103=CARTESIAN_POINT('Ctrl Pts',(-30.9422610583467,-0.863842203589976,
313.630365835055));
#16104=CARTESIAN_POINT('Ctrl Pts',(-30.9162831050408,-0.774168418976915,
313.635397004374));
#16105=CARTESIAN_POINT('Ctrl Pts',(-30.894629836595,-0.683518719038402,
313.640428173694));
#16106=CARTESIAN_POINT('Ctrl Pts',(-30.87295256024,-0.592768511882588,313.645464921287));
#16107=CARTESIAN_POINT('Ctrl Pts',(-30.8556096435039,-0.501040663057724,
313.65050166888));
#16108=CARTESIAN_POINT('Ctrl Pts',(-30.8426652447765,-0.408784116222606,
313.655538416473));
#16109=CARTESIAN_POINT('Ctrl Pts',(-30.8297128350154,-0.316470473626301,
313.660578281209));
#16110=CARTESIAN_POINT('Ctrl Pts',(-30.8211644029398,-0.223627924458978,
313.665618145946));
#16111=CARTESIAN_POINT('Ctrl Pts',(-30.817032060154,-0.130708783571081,
313.670658010683));
#16112=CARTESIAN_POINT('Ctrl Pts',(-30.8128929650379,-0.0376378109597996,
313.675706110659));
#16113=CARTESIAN_POINT('Ctrl Pts',(-30.8131843633999,0.0555095587920874,
313.680754210635));
#16114=CARTESIAN_POINT('Ctrl Pts',(-30.8178662867567,0.148282947718572,
313.685802310612));
#16115=CARTESIAN_POINT('Ctrl Pts',(-30.820273519263,0.195982813891284,313.688397814517));
#16116=CARTESIAN_POINT('Ctrl Pts',(-30.8238405673749,0.243583925396814,
313.690993318422));
#16117=CARTESIAN_POINT('Ctrl Pts',(-30.8285567317385,0.291026075299615,
313.693588822328));
#16118=CARTESIAN_POINT('Ctrl Pts',(-30.8377518180949,0.383523840785478,
313.698649265669));
#16119=CARTESIAN_POINT('Ctrl Pts',(-30.8513511994363,0.475748885997435,
313.70370970901));
#16120=CARTESIAN_POINT('Ctrl Pts',(-30.8693308450819,0.567249340346028,
313.708770152352));
#16121=CARTESIAN_POINT('Ctrl Pts',(-30.8872856905938,0.658623584003588,
313.713823615596));
#16122=CARTESIAN_POINT('Ctrl Pts',(-30.9096087087805,0.749274792323898,
313.71887707884));
#16123=CARTESIAN_POINT('Ctrl Pts',(-30.9362240836932,0.838755864454321,
313.723930542084));
#16124=CARTESIAN_POINT('Ctrl Pts',(-30.9628108991636,0.92814091954475,313.728978582745));
#16125=CARTESIAN_POINT('Ctrl Pts',(-30.9936807902049,1.01635791227163,313.734026623405));
#16126=CARTESIAN_POINT('Ctrl Pts',(-31.0287070506272,1.10297066234205,313.739074664066));
#16127=CARTESIAN_POINT('Ctrl Pts',(-31.0637076319269,1.18951991321485,313.744119003811));
#16128=CARTESIAN_POINT('Ctrl Pts',(-31.1028583595386,1.27446685025617,313.749163343555));
#16129=CARTESIAN_POINT('Ctrl Pts',(-31.1459832547663,1.35739216785919,313.7542076833));
#16130=CARTESIAN_POINT('Ctrl Pts',(-31.1890921057858,1.4402866338845,313.759250146345));
#16131=CARTESIAN_POINT('Ctrl Pts',(-31.2361719827669,1.52116058245747,313.764292609391));
#16132=CARTESIAN_POINT('Ctrl Pts',(-31.2869999383912,1.59961727575772,313.769335072437));
#16133=CARTESIAN_POINT('Ctrl Pts',(-31.3378230805654,1.67806653914332,313.774377057957));
#16134=CARTESIAN_POINT('Ctrl Pts',(-31.3923933547688,1.75409863099902,313.779419043477));
#16135=CARTESIAN_POINT('Ctrl Pts',(-31.4504438762798,1.82734485429543,313.784461028998));
#16136=CARTESIAN_POINT('Ctrl Pts',(-31.5085049997242,1.9006044547598,313.78950393535));
#16137=CARTESIAN_POINT('Ctrl Pts',(-31.570047357575,1.97107682948833,313.794546841703));
#16138=CARTESIAN_POINT('Ctrl Pts',(-31.6347638098422,2.0384263803931,313.799589748055));
#16139=CARTESIAN_POINT('Ctrl Pts',(-31.699549382117,2.10584786357019,313.804638040453));
#16140=CARTESIAN_POINT('Ctrl Pts',(-31.7675155087973,2.17013954534008,313.80968633285));
#16141=CARTESIAN_POINT('Ctrl Pts',(-31.8383184347808,2.23100296061964,313.814734625248));
#16142=CARTESIAN_POINT('Ctrl Pts',(-31.9091637838538,2.2919028435179,313.819785942438));
#16143=CARTESIAN_POINT('Ctrl Pts',(-31.9828489677308,2.34937009781821,313.824837259628));
#16144=CARTESIAN_POINT('Ctrl Pts',(-32.0589991408942,2.40314813195443,313.829888576818));
#16145=CARTESIAN_POINT('Ctrl Pts',(-32.1352696270824,2.45701113238409,313.834947874808));
#16146=CARTESIAN_POINT('Ctrl Pts',(-32.2140125048864,2.50717303817611,313.840007172797));
#16147=CARTESIAN_POINT('Ctrl Pts',(-32.2948262826152,2.55342204493357,313.845066470786));
#16148=CARTESIAN_POINT('Ctrl Pts',(-32.3344062686011,2.57607331914408,313.847544352023));
#16149=CARTESIAN_POINT('Ctrl Pts',(-32.3744826658589,2.59778671489475,313.85002223326));
#16150=CARTESIAN_POINT('Ctrl Pts',(-32.4150065832655,2.61854157119393,313.852500114497));
#16151=CARTESIAN_POINT('Ctrl Pts',(-32.4967291453233,2.66039685420849,313.857497133939));
#16152=CARTESIAN_POINT('Ctrl Pts',(-32.5805737516244,2.69850485920996,313.862494153382));
#16153=CARTESIAN_POINT('Ctrl Pts',(-32.6661578794082,2.73264180987857,313.867491172824));
#16154=CARTESIAN_POINT('Ctrl Pts',(-32.7516251033333,2.76673213109187,313.872481366575));
#16155=CARTESIAN_POINT('Ctrl Pts',(-32.8388267110154,2.79686200405708,313.877471560325));
#16156=CARTESIAN_POINT('Ctrl Pts',(-32.9273556718184,2.82285352856265,313.882461754076));
#16157=CARTESIAN_POINT('Ctrl Pts',(-33.0157868439752,2.84881634296056,313.887446435684));
#16158=CARTESIAN_POINT('Ctrl Pts',(-33.1055420212523,2.8706497665468,313.892431117291));
#16159=CARTESIAN_POINT('Ctrl Pts',(-33.1961955297968,2.88822449272751,313.897415798899));
#16160=CARTESIAN_POINT('Ctrl Pts',(-33.2867944662325,2.90578863917572,313.9023974798));
#16161=CARTESIAN_POINT('Ctrl Pts',(-33.3782902151584,2.91909909095568,313.907379160701));
#16162=CARTESIAN_POINT('Ctrl Pts',(-33.470244304611,2.92807702597382,313.912360841602));
#16163=CARTESIAN_POINT('Ctrl Pts',(-33.5621701181447,2.93705220027338,313.917340990635));
#16164=CARTESIAN_POINT('Ctrl Pts',(-33.654553539928,2.94169745945905,313.922321139667));
#16165=CARTESIAN_POINT('Ctrl Pts',(-33.7469496049711,2.94198568571584,313.927301288699));
#16166=CARTESIAN_POINT('Ctrl Pts',(-33.8393444666851,2.94227390821889,313.932281372872));
#16167=CARTESIAN_POINT('Ctrl Pts',(-33.9317515164511,2.93820521068346,313.937261457044));
#16168=CARTESIAN_POINT('Ctrl Pts',(-34.0237257062877,2.92980459176221,313.942241541217));
#16169=CARTESIAN_POINT('Ctrl Pts',(-34.1157841649718,2.92139627600259,313.947226188257));
#16170=CARTESIAN_POINT('Ctrl Pts',(-34.2074085176988,2.90864815316715,313.952210835296));
#16171=CARTESIAN_POINT('Ctrl Pts',(-34.2981592111505,2.89163709850599,313.957195482335));
#16172=CARTESIAN_POINT('Ctrl Pts',(-34.3889512416492,2.87461829528955,313.962182399887));
#16173=CARTESIAN_POINT('Ctrl Pts',(-34.4788683776911,2.85333279921205,313.967169317439));
#16174=CARTESIAN_POINT('Ctrl Pts',(-34.5674838877613,2.82790806810761,313.972156234991));
#16175=CARTESIAN_POINT('Ctrl Pts',(-34.6562458761417,2.80244131082011,313.977151395741));
#16176=CARTESIAN_POINT('Ctrl Pts',(-34.743701509796,2.77282179832228,313.982146556492));
#16177=CARTESIAN_POINT('Ctrl Pts',(-34.8294418839185,2.73922602466058,313.987141717242));
#16178=CARTESIAN_POINT('Ctrl Pts',(-34.9026418061714,2.71054399422586,313.991406282009));
#16179=CARTESIAN_POINT('Ctrl Pts',(-34.9745917256034,2.67896467102844,313.995670846776));
#16180=CARTESIAN_POINT('Ctrl Pts',(-35.0450520381518,2.64462403965778,313.999935411543));
#16181=CARTESIAN_POINT('',(-32.4672051712042,2.64462557919705,314.));
#16182=CARTESIAN_POINT('Origin',(-33.7561270252576,0.,314.));
#16183=CARTESIAN_POINT('',(-36.6981257223057,-0.00276885671560002,313.32217611709));
#16184=CARTESIAN_POINT('Ctrl Pts',(-32.4672051712041,2.64462557919703,314.));
#16185=CARTESIAN_POINT('Ctrl Pts',(-31.5870128673401,2.21564269967557,313.947029569277));
#16186=CARTESIAN_POINT('Ctrl Pts',(-30.3047647042133,0.41477504708739,313.841088707831));
#16187=CARTESIAN_POINT('Ctrl Pts',(-31.5376353324677,-2.68170030602472,
313.682177415661));
#16188=CARTESIAN_POINT('Ctrl Pts',(-34.8089410995756,-3.31499725615595,
313.523266123492));
#16189=CARTESIAN_POINT('Ctrl Pts',(-36.5488387827353,-1.49996772299205,
313.403265827269));
#16190=CARTESIAN_POINT('Ctrl Pts',(-36.6995965658053,-0.262825748460331,
313.33623596177));
#16191=CARTESIAN_POINT('Ctrl Pts',(-36.6972963689876,-0.00277565787605923,
313.322176526993));
#16192=CARTESIAN_POINT('',(-36.6981268796127,0.000925729196293329,312.322176117046));
#16193=CARTESIAN_POINT('Ctrl Pts',(-36.6981257223057,-0.00276885671560002,
313.32217611709));
#16194=CARTESIAN_POINT('Ctrl Pts',(-36.6982125227697,0.0894594086611232,
313.31719121744));
#16195=CARTESIAN_POINT('Ctrl Pts',(-36.693958203422,0.181789992050611,313.312206317791));
#16196=CARTESIAN_POINT('Ctrl Pts',(-36.6853606860934,0.273777574367638,
313.307221418141));
#16197=CARTESIAN_POINT('Ctrl Pts',(-36.6767677068704,0.365716602043123,
313.302239149716));
#16198=CARTESIAN_POINT('Ctrl Pts',(-36.6638361227904,0.457312536473602,
313.297256881291));
#16199=CARTESIAN_POINT('Ctrl Pts',(-36.6466158988542,0.548122314464703,
313.292274612867));
#16200=CARTESIAN_POINT('Ctrl Pts',(-36.629399700581,0.638910863372949,313.287293509173));
#16201=CARTESIAN_POINT('Ctrl Pts',(-36.6078969383671,0.728913174457869,
313.28231240548));
#16202=CARTESIAN_POINT('Ctrl Pts',(-36.5822089723762,0.8176948258185,313.277331301786));
#16203=CARTESIAN_POINT('Ctrl Pts',(-36.5565194576737,0.90648182976984,313.272349897785));
#16204=CARTESIAN_POINT('Ctrl Pts',(-36.5266443659156,0.994047591601018,
313.267368493784));
#16205=CARTESIAN_POINT('Ctrl Pts',(-36.4927350019615,1.07997258383734,313.262387089783));
#16206=CARTESIAN_POINT('Ctrl Pts',(-36.4587912382054,1.16598474381675,313.257400632331));
#16207=CARTESIAN_POINT('Ctrl Pts',(-36.4208051973971,1.25035238688473,313.252414174879));
#16208=CARTESIAN_POINT('Ctrl Pts',(-36.3789763092459,1.33267611724752,313.247427717427));
#16209=CARTESIAN_POINT('Ctrl Pts',(-36.3371257405411,1.41504251726122,313.242438675418));
#16210=CARTESIAN_POINT('Ctrl Pts',(-36.2914285852409,1.49536250107787,313.237449633408));
#16211=CARTESIAN_POINT('Ctrl Pts',(-36.2421290349298,1.57326348966281,313.232460591399));
#16212=CARTESIAN_POINT('Ctrl Pts',(-36.1927449189176,1.65129810526203,313.227462991465));
#16213=CARTESIAN_POINT('Ctrl Pts',(-36.1397463285022,1.72690506679231,313.222465391531));
#16214=CARTESIAN_POINT('Ctrl Pts',(-36.0834192937624,1.79974295302352,313.217467791597));
#16215=CARTESIAN_POINT('Ctrl Pts',(-36.0382449104581,1.85815906895937,313.213459707449));
#16216=CARTESIAN_POINT('Ctrl Pts',(-35.9909305000231,1.91479467579664,313.209451623302));
#16217=CARTESIAN_POINT('Ctrl Pts',(-35.9416403734495,1.96949115379456,313.205443539154));
#16218=CARTESIAN_POINT('Ctrl Pts',(-35.8795065263467,2.03844010639887,313.200391052887));
#16219=CARTESIAN_POINT('Ctrl Pts',(-35.8139951039231,2.10456965393969,313.195338566621));
#16220=CARTESIAN_POINT('Ctrl Pts',(-35.745392031301,2.16753056166023,313.190286080354));
#16221=CARTESIAN_POINT('Ctrl Pts',(-35.6768836489419,2.23040456678762,313.185240567845));
#16222=CARTESIAN_POINT('Ctrl Pts',(-35.6052924204783,2.2901183251654,313.180195055337));
#16223=CARTESIAN_POINT('Ctrl Pts',(-35.5309432084145,2.34635707342348,313.175149542828));
#16224=CARTESIAN_POINT('Ctrl Pts',(-35.456673650143,2.40253557047714,313.170109435814));
#16225=CARTESIAN_POINT('Ctrl Pts',(-35.3796523336779,2.45524619078854,313.165069328799));
#16226=CARTESIAN_POINT('Ctrl Pts',(-35.3002386850107,2.50421308642343,313.160029221784));
#16227=CARTESIAN_POINT('Ctrl Pts',(-35.2208824331836,2.55314459084892,313.154992757547));
#16228=CARTESIAN_POINT('Ctrl Pts',(-35.139137662988,2.59833751633471,313.149956293309));
#16229=CARTESIAN_POINT('Ctrl Pts',(-35.0553935274371,2.63955878061359,313.144919829072));
#16230=CARTESIAN_POINT('Ctrl Pts',(-34.9716799452144,2.68076500566842,313.139885202345));
#16231=CARTESIAN_POINT('Ctrl Pts',(-34.8859688449188,2.718002252192,313.134850575618));
#16232=CARTESIAN_POINT('Ctrl Pts',(-34.7986738552168,2.75108344245354,313.129815948891));
#16233=CARTESIAN_POINT('Ctrl Pts',(-34.7113862993168,2.7841618156116,313.124781750899));
#16234=CARTESIAN_POINT('Ctrl Pts',(-34.6225155376344,2.81308467893449,313.119747552907));
#16235=CARTESIAN_POINT('Ctrl Pts',(-34.5324939711156,2.83771358057489,313.114713354915));
#16236=CARTESIAN_POINT('Ctrl Pts',(-34.4424548932985,2.86234727311215,313.109678177654));
#16237=CARTESIAN_POINT('Ctrl Pts',(-34.351264994605,2.88268522825309,313.104643000393));
#16238=CARTESIAN_POINT('Ctrl Pts',(-34.2593694646226,2.89863951660464,313.099607823132));
#16239=CARTESIAN_POINT('Ctrl Pts',(-34.1673731693013,2.91461129916153,313.094567124695));
#16240=CARTESIAN_POINT('Ctrl Pts',(-34.074670136559,2.92618974390358,313.089526426259));
#16241=CARTESIAN_POINT('Ctrl Pts',(-33.9817130180977,2.93333853481563,313.084485727822));
#16242=CARTESIAN_POINT('Ctrl Pts',(-33.8886989041882,2.94049170891586,313.079441938747));
#16243=CARTESIAN_POINT('Ctrl Pts',(-33.7954308381143,2.94320980922228,313.074398149672));
#16244=CARTESIAN_POINT('Ctrl Pts',(-33.7023616329589,2.94150867457347,313.069354360596));
#16245=CARTESIAN_POINT('Ctrl Pts',(-33.6091419391262,2.9398047892672,313.064302415943));
#16246=CARTESIAN_POINT('Ctrl Pts',(-33.5161221908488,2.93366743266693,313.05925047129));
#16247=CARTESIAN_POINT('Ctrl Pts',(-33.4237500611861,2.92316430495355,313.054198526637));
#16248=CARTESIAN_POINT('Ctrl Pts',(-33.3770254414711,2.91785150497788,313.051643100086));
#16249=CARTESIAN_POINT('Ctrl Pts',(-33.3304663662841,2.91142247559488,313.049087673535));
#16250=CARTESIAN_POINT('Ctrl Pts',(-33.2841295196668,2.90389089924469,313.046532246984));
#16251=CARTESIAN_POINT('Ctrl Pts',(-33.1925050259082,2.88899828309429,313.041479256088));
#16252=CARTESIAN_POINT('Ctrl Pts',(-33.1014221356118,2.86973832244506,313.036426265192));
#16253=CARTESIAN_POINT('Ctrl Pts',(-33.0113293612816,2.84616240572037,313.031373274297));
#16254=CARTESIAN_POINT('Ctrl Pts',(-32.9213605804438,2.82261893621768,313.026327237765));
#16255=CARTESIAN_POINT('Ctrl Pts',(-32.8323796336531,2.79477142573066,313.021281201234));
#16256=CARTESIAN_POINT('Ctrl Pts',(-32.7448271219679,2.76272266172453,313.016235164703));
#16257=CARTESIAN_POINT('Ctrl Pts',(-32.6573680776615,2.73070811163078,313.011194515108));
#16258=CARTESIAN_POINT('Ctrl Pts',(-32.5713348522062,2.69450137472164,313.006153865513));
#16259=CARTESIAN_POINT('Ctrl Pts',(-32.487154032446,2.65425536516644,313.001113215918));
#16260=CARTESIAN_POINT('Ctrl Pts',(-32.403033623576,2.61403823745473,312.996076183657));
#16261=CARTESIAN_POINT('Ctrl Pts',(-32.3207633776623,2.56978778971267,312.991039151396));
#16262=CARTESIAN_POINT('Ctrl Pts',(-32.2407500152919,2.52170508142155,312.986002119135));
#16263=CARTESIAN_POINT('Ctrl Pts',(-32.1607655941159,2.47363976486316,312.980966908792));
#16264=CARTESIAN_POINT('Ctrl Pts',(-32.0830368150351,2.421745170032,312.975931698448));
#16265=CARTESIAN_POINT('Ctrl Pts',(-32.0079449655349,2.36626783903762,312.970896488104));
#16266=CARTESIAN_POINT('Ctrl Pts',(-31.9328592875401,2.31079506750807,312.965861691585));
#16267=CARTESIAN_POINT('Ctrl Pts',(-31.8604104653208,2.25174040930801,312.960826895065));
#16268=CARTESIAN_POINT('Ctrl Pts',(-31.7909490631511,2.1893925132901,312.955792098546));
#16269=CARTESIAN_POINT('Ctrl Pts',(-31.7214739542515,2.12703231424149,312.950756308517));
#16270=CARTESIAN_POINT('Ctrl Pts',(-31.6549877664083,2.06137788365821,312.945720518487));
#16271=CARTESIAN_POINT('Ctrl Pts',(-31.5918055080642,1.9927559735737,312.940684728458));
#16272=CARTESIAN_POINT('Ctrl Pts',(-31.5285537517061,1.92405858207097,312.935643399256));
#16273=CARTESIAN_POINT('Ctrl Pts',(-31.468613480408,1.85238752273233,312.930602070055));
#16274=CARTESIAN_POINT('Ctrl Pts',(-31.4122603478211,1.77810376480194,312.925560740853));
#16275=CARTESIAN_POINT('Ctrl Pts',(-31.3558725424498,1.70377430178639,312.920516309838));
#16276=CARTESIAN_POINT('Ctrl Pts',(-31.3030765207695,1.62682930579491,312.915471878823));
#16277=CARTESIAN_POINT('Ctrl Pts',(-31.2541041736667,1.54765811796957,312.910427447807));
#16278=CARTESIAN_POINT('Ctrl Pts',(-31.2050525418011,1.46835875436285,312.905374850009));
#16279=CARTESIAN_POINT('Ctrl Pts',(-31.1598371580439,1.38682639159117,312.900322252211));
#16280=CARTESIAN_POINT('Ctrl Pts',(-31.1186435280827,1.30347412790968,312.895269654413));
#16281=CARTESIAN_POINT('Ctrl Pts',(-31.0978570130047,1.26141415195149,312.892720087881));
#16282=CARTESIAN_POINT('Ctrl Pts',(-31.0780937735029,1.21889108890137,312.890170521348));
#16283=CARTESIAN_POINT('Ctrl Pts',(-31.0593728666175,1.17595961149077,312.887620954815));
#16284=CARTESIAN_POINT('Ctrl Pts',(-31.0222781243352,1.09089257386798,312.88256908879));
#16285=CARTESIAN_POINT('Ctrl Pts',(-30.9891457010024,1.00391569124036,312.877517222764));
#16286=CARTESIAN_POINT('Ctrl Pts',(-30.9601754184417,0.91543356522659,312.872465356738));
#16287=CARTESIAN_POINT('Ctrl Pts',(-30.9312451269952,0.827073581577323,
312.867420464402));
#16288=CARTESIAN_POINT('Ctrl Pts',(-30.9064656964087,0.73721290211214,312.862375572066));
#16289=CARTESIAN_POINT('Ctrl Pts',(-30.8859894678776,0.646277341175262,
312.857330679729));
#16290=CARTESIAN_POINT('Ctrl Pts',(-30.865535175313,0.555439198540542,312.852291191933));
#16291=CARTESIAN_POINT('Ctrl Pts',(-30.8493750189145,0.463528894372842,
312.847251704136));
#16292=CARTESIAN_POINT('Ctrl Pts',(-30.8376116192949,0.370987634778209,
312.842212216339));
#16293=CARTESIAN_POINT('Ctrl Pts',(-30.8258567132236,0.278513192913623,
312.837176367213));
#16294=CARTESIAN_POINT('Ctrl Pts',(-30.8184923098604,0.185409140651498,
312.832140518087));
#16295=CARTESIAN_POINT('Ctrl Pts',(-30.8155698016233,0.0921260795430611,
312.82710466896));
#16296=CARTESIAN_POINT('Ctrl Pts',(-30.8126483581473,-0.00112299562917563,
312.822070654551));
#16297=CARTESIAN_POINT('Ctrl Pts',(-30.8141656087479,-0.0945505064111075,
312.817036640142));
#16298=CARTESIAN_POINT('Ctrl Pts',(-30.8201209384099,-0.187702578546671,
312.812002625733));
#16299=CARTESIAN_POINT('Ctrl Pts',(-30.8260757651075,-0.280846783415015,
312.806969036478));
#16300=CARTESIAN_POINT('Ctrl Pts',(-30.8364678971054,-0.373715152463849,
312.801935447222));
#16301=CARTESIAN_POINT('Ctrl Pts',(-30.8512446824128,-0.465856817303986,
312.796901857967));
#16302=CARTESIAN_POINT('Ctrl Pts',(-30.8660243553348,-0.558016488064301,
312.79186728507));
#16303=CARTESIAN_POINT('Ctrl Pts',(-30.8851903124993,-0.649448733936276,
312.786832712172));
#16304=CARTESIAN_POINT('Ctrl Pts',(-30.9086386116362,-0.739711926557905,
312.781798139275));
#16305=CARTESIAN_POINT('Ctrl Pts',(-30.9321126738784,-0.830074293116133,
312.776758034794));
#16306=CARTESIAN_POINT('Ctrl Pts',(-30.9598783581177,-0.91926461175442,
312.771717930312));
#16307=CARTESIAN_POINT('Ctrl Pts',(-30.9917816403831,-1.00685579559491,
312.766677825831));
#16308=CARTESIAN_POINT('Ctrl Pts',(-31.0237045179241,-1.09450077870813,
312.761634625674));
#16309=CARTESIAN_POINT('Ctrl Pts',(-31.0597698811519,-1.18054426216621,
312.756591425516));
#16310=CARTESIAN_POINT('Ctrl Pts',(-31.0997761506711,-1.26458057516464,
312.751548225359));
#16311=CARTESIAN_POINT('Ctrl Pts',(-31.1398472244555,-1.34875301461476,
312.746496855959));
#16312=CARTESIAN_POINT('Ctrl Pts',(-31.1838717391617,-1.43091140158479,
312.74144548656));
#16313=CARTESIAN_POINT('Ctrl Pts',(-31.2316030189279,-1.51067618683325,
312.736394117161));
#16314=CARTESIAN_POINT('Ctrl Pts',(-31.2558069406338,-1.5511238896079,312.733832632323));
#16315=CARTESIAN_POINT('Ctrl Pts',(-31.280963330977,-1.59095659018532,312.731271147484));
#16316=CARTESIAN_POINT('Ctrl Pts',(-31.3070360320273,-1.63012800321881,
312.728709662646));
#16317=CARTESIAN_POINT('Ctrl Pts',(-31.358462392419,-1.70739054689708,312.723657334458));
#16318=CARTESIAN_POINT('Ctrl Pts',(-31.4136407908189,-1.7823558205591,312.71860500627));
#16319=CARTESIAN_POINT('Ctrl Pts',(-31.4723392186545,-1.85463669067852,
312.713552678083));
#16320=CARTESIAN_POINT('Ctrl Pts',(-31.530956689728,-1.92681787115682,312.708507318057));
#16321=CARTESIAN_POINT('Ctrl Pts',(-31.5930842654704,-1.99632166322212,
312.703461958031));
#16322=CARTESIAN_POINT('Ctrl Pts',(-31.6584463952587,-2.06278936746514,
312.698416598005));
#16323=CARTESIAN_POINT('Ctrl Pts',(-31.7237385724353,-2.12918593587593,
312.693376637682));
#16324=CARTESIAN_POINT('Ctrl Pts',(-31.7922581131499,-2.19255255992412,
312.68833667736));
#16325=CARTESIAN_POINT('Ctrl Pts',(-31.8636896051547,-2.2525640081903,312.683296717037));
#16326=CARTESIAN_POINT('Ctrl Pts',(-31.9350695999261,-2.31253219229558,
312.678260390182));
#16327=CARTESIAN_POINT('Ctrl Pts',(-32.0093570341332,-2.36914972349256,
312.673224063327));
#16328=CARTESIAN_POINT('Ctrl Pts',(-32.0862008578061,-2.42212935147171,
312.668187736472));
#16329=CARTESIAN_POINT('Ctrl Pts',(-32.1630167340359,-2.4750897112122,312.663153241286));
#16330=CARTESIAN_POINT('Ctrl Pts',(-32.2423867873326,-2.5244145442575,312.6581187461));
#16331=CARTESIAN_POINT('Ctrl Pts',(-32.3239290548795,-2.56985855129127,
312.653084250914));
#16332=CARTESIAN_POINT('Ctrl Pts',(-32.4054644760275,-2.61529874278482,
312.648050178432));
#16333=CARTESIAN_POINT('Ctrl Pts',(-32.489171360666,-2.65685854000789,312.643016105949));
#16334=CARTESIAN_POINT('Ctrl Pts',(-32.5746420944852,-2.69433801857853,
312.637982033466));
#16335=CARTESIAN_POINT('Ctrl Pts',(-32.6601295605093,-2.73182483433104,
312.632946975486));
#16336=CARTESIAN_POINT('Ctrl Pts',(-32.7473811545089,-2.76522956698514,
312.627911917506));
#16337=CARTESIAN_POINT('Ctrl Pts',(-32.835969254871,-2.79440041468597,312.622876859527));
#16338=CARTESIAN_POINT('Ctrl Pts',(-32.9246546767038,-2.82360330901372,
312.617836270113));
#16339=CARTESIAN_POINT('Ctrl Pts',(-33.0146791131183,-2.84856289472312,
312.612795680699));
#16340=CARTESIAN_POINT('Ctrl Pts',(-33.1056000456081,-2.86917734703662,
312.607755091285));
#16341=CARTESIAN_POINT('Ctrl Pts',(-33.1965768286452,-2.88980446231358,
312.602711405558));
#16342=CARTESIAN_POINT('Ctrl Pts',(-33.2884507669756,-2.90608105307196,
312.597667719831));
#16343=CARTESIAN_POINT('Ctrl Pts',(-33.3807715909833,-2.91795687047645,
312.592624034104));
#16344=CARTESIAN_POINT('Ctrl Pts',(-33.473241877852,-2.92985191424364,312.587572182899));
#16345=CARTESIAN_POINT('Ctrl Pts',(-33.5661600524894,-2.9373319255915,312.582520331693));
#16346=CARTESIAN_POINT('Ctrl Pts',(-33.6590733812322,-2.94039871279073,
312.577468480488));
#16347=CARTESIAN_POINT('Ctrl Pts',(-33.7060961077578,-2.94195079038533,
312.574911777151));
#16348=CARTESIAN_POINT('Ctrl Pts',(-33.7531176306962,-2.94237334144602,
312.572355073813));
#16349=CARTESIAN_POINT('Ctrl Pts',(-33.8000797915366,-2.9416716598452,312.569798370476));
#16350=CARTESIAN_POINT('Ctrl Pts',(-33.8928824666442,-2.94028505564163,
312.56474602823));
#16351=CARTESIAN_POINT('Ctrl Pts',(-33.985785988718,-2.93450010495286,312.559693685985));
#16352=CARTESIAN_POINT('Ctrl Pts',(-34.0783392594271,-2.9243021861893,312.554641343739));
#16353=CARTESIAN_POINT('Ctrl Pts',(-34.1707649080661,-2.91411832937615,
312.549595968188));
#16354=CARTESIAN_POINT('Ctrl Pts',(-34.2628408273101,-2.89953364451495,
312.544550592637));
#16355=CARTESIAN_POINT('Ctrl Pts',(-34.3541162411757,-2.88058551298961,
312.539505217086));
#16356=CARTESIAN_POINT('Ctrl Pts',(-34.445293995534,-2.86165765488854,312.5344652398));
#16357=CARTESIAN_POINT('Ctrl Pts',(-34.5356725142954,-2.838375719569,312.529425262514));
#16358=CARTESIAN_POINT('Ctrl Pts',(-34.6248075687399,-2.81082872359299,
312.524385285228));
#16359=CARTESIAN_POINT('Ctrl Pts',(-34.7138783998947,-2.78330157568583,
312.51934893933));
#16360=CARTESIAN_POINT('Ctrl Pts',(-34.8017071243158,-2.75151560602708,
312.514312593432));
#16361=CARTESIAN_POINT('Ctrl Pts',(-34.8878621418458,-2.7156103597315,312.509276247533));
#16362=CARTESIAN_POINT('Ctrl Pts',(-34.9739858476426,-2.67971816265264,
312.504241732019));
#16363=CARTESIAN_POINT('Ctrl Pts',(-35.0584366453236,-2.63970983378514,
312.499207216504));
#16364=CARTESIAN_POINT('Ctrl Pts',(-35.1408014596098,-2.59577362473145,
312.494172700989));
#16365=CARTESIAN_POINT('Ctrl Pts',(-35.2231593791528,-2.55184109356958,
312.489138606912));
#16366=CARTESIAN_POINT('Ctrl Pts',(-35.3034312706049,-2.50398154520596,
312.484104512836));
#16367=CARTESIAN_POINT('Ctrl Pts',(-35.3812283112679,-2.45242936905584,
312.479070418759));
#16368=CARTESIAN_POINT('Ctrl Pts',(-35.4590406010642,-2.40086708807403,
312.474035337941));
#16369=CARTESIAN_POINT('Ctrl Pts',(-35.534376706569,-2.34561098752187,312.469000257123));
#16370=CARTESIAN_POINT('Ctrl Pts',(-35.6068774241292,-2.28693833783874,
312.463965176305));
#16371=CARTESIAN_POINT('Ctrl Pts',(-35.6794578148327,-2.22820121107752,
312.458924562291));
#16372=CARTESIAN_POINT('Ctrl Pts',(-35.7491962520428,-2.1660403205648,312.453883948276));
#16373=CARTESIAN_POINT('Ctrl Pts',(-35.8157674776937,-2.1007725261648,312.448843334262));
#16374=CARTESIAN_POINT('Ctrl Pts',(-35.8823796099752,-2.03546462606553,
312.443799622895));
#16375=CARTESIAN_POINT('Ctrl Pts',(-35.9458203543912,-1.96704634688947,
312.438755911528));
#16376=CARTESIAN_POINT('Ctrl Pts',(-36.005803612625,-1.89586899659519,312.433712200161));
#16377=CARTESIAN_POINT('Ctrl Pts',(-36.0658839966621,-1.82457639485368,
312.42866032194));
#16378=CARTESIAN_POINT('Ctrl Pts',(-36.122495448521,-1.75051615561669,312.42360844372));
#16379=CARTESIAN_POINT('Ctrl Pts',(-36.1753942973603,-1.67406985103148,
312.418556565499));
#16380=CARTESIAN_POINT('Ctrl Pts',(-36.2021636839723,-1.63538430820029,
312.416000069768));
#16381=CARTESIAN_POINT('Ctrl Pts',(-36.2279830463466,-1.59608814747113,
312.413443574037));
#16382=CARTESIAN_POINT('Ctrl Pts',(-36.2528253442714,-1.55623311358982,
312.410887078307));
#16383=CARTESIAN_POINT('Ctrl Pts',(-36.3032815210905,-1.47528518185132,
312.405694684229));
#16384=CARTESIAN_POINT('Ctrl Pts',(-36.3498771649948,-1.39175301603299,
312.400502290151));
#16385=CARTESIAN_POINT('Ctrl Pts',(-36.3923463531807,-1.30602896410628,
312.395309896074));
#16386=CARTESIAN_POINT('Ctrl Pts',(-36.4347463756819,-1.22044452310699,
312.390125958374));
#16387=CARTESIAN_POINT('Ctrl Pts',(-36.4730331292883,-1.13267566198725,
312.384942020674));
#16388=CARTESIAN_POINT('Ctrl Pts',(-36.5069847334643,-1.04314230534479,
312.379758082974));
#16389=CARTESIAN_POINT('Ctrl Pts',(-36.5408749019281,-0.953770960061013,
312.374583525652));
#16390=CARTESIAN_POINT('Ctrl Pts',(-36.5704453987093,-0.86264185998207,
312.369408968331));
#16391=CARTESIAN_POINT('Ctrl Pts',(-36.5955214651476,-0.770196867509516,
312.364234411009));
#16392=CARTESIAN_POINT('Ctrl Pts',(-36.6205707907295,-0.677850457415516,
312.359065371782));
#16393=CARTESIAN_POINT('Ctrl Pts',(-36.6411351109393,-0.58419134043354,
312.353896332555));
#16394=CARTESIAN_POINT('Ctrl Pts',(-36.6570887399773,-0.489678598399612,
312.348727293328));
#16395=CARTESIAN_POINT('Ctrl Pts',(-36.6730258748099,-0.395263571598767,
312.343563598289));
#16396=CARTESIAN_POINT('Ctrl Pts',(-36.6843617411924,-0.299997080946183,
312.33839990325));
#16397=CARTESIAN_POINT('Ctrl Pts',(-36.6910214454844,-0.204349558652154,
312.333236208211));
#16398=CARTESIAN_POINT('Ctrl Pts',(-36.6957762406295,-0.136060584442952,
312.32954951117));
#16399=CARTESIAN_POINT('Ctrl Pts',(-36.6981484348598,-0.0675776627360847,
312.32586281413));
#16400=CARTESIAN_POINT('Ctrl Pts',(-36.698126879613,0.000925728376547487,
312.32217611709));
#16401=CARTESIAN_POINT('',(-36.6981261623761,0.00225326298871394,311.322176117122));
#16402=CARTESIAN_POINT('Ctrl Pts',(-36.6981268796127,0.000925729196304501,
312.322176117046));
#16403=CARTESIAN_POINT('Ctrl Pts',(-36.6980951904088,0.101635130789933,
312.316756165613));
#16404=CARTESIAN_POINT('Ctrl Pts',(-36.6928881286928,0.202195227316754,
312.311336214181));
#16405=CARTESIAN_POINT('Ctrl Pts',(-36.6825766586399,0.30208697965426,312.305916262748));
#16406=CARTESIAN_POINT('Ctrl Pts',(-36.6722226572952,0.402390751348661,
312.300473955868));
#16407=CARTESIAN_POINT('Ctrl Pts',(-36.6567221512165,0.502020334260477,
312.295031648987));
#16408=CARTESIAN_POINT('Ctrl Pts',(-36.6361975885368,0.600464445685857,
312.289589342106));
#16409=CARTESIAN_POINT('Ctrl Pts',(-36.6156282772227,0.699123189676856,
312.284135169647));
#16410=CARTESIAN_POINT('Ctrl Pts',(-36.5900131202047,0.796590984724717,
312.278680997189));
#16411=CARTESIAN_POINT('Ctrl Pts',(-36.5595242514719,0.892372115237896,
312.27322682473));
#16412=CARTESIAN_POINT('Ctrl Pts',(-36.5289401958915,0.988452276323434,
312.267755624237));
#16413=CARTESIAN_POINT('Ctrl Pts',(-36.4934521105363,1.08283493328951,312.262284423745));
#16414=CARTESIAN_POINT('Ctrl Pts',(-36.4532806102076,1.17504320737213,312.256813223253));
#16415=CARTESIAN_POINT('Ctrl Pts',(-36.4414412154882,1.20221894500509,312.255200744214));
#16416=CARTESIAN_POINT('Ctrl Pts',(-36.4291953163461,1.22920598503843,312.253588265176));
#16417=CARTESIAN_POINT('Ctrl Pts',(-36.4165493003502,1.25599256295217,312.251975786138));
#16418=CARTESIAN_POINT('Ctrl Pts',(-36.3769262856362,1.33992136481035,312.246923500842));
#16419=CARTESIAN_POINT('Ctrl Pts',(-36.3332566812781,1.42212398347406,312.241871215547));
#16420=CARTESIAN_POINT('Ctrl Pts',(-36.2857136239563,1.50218362382368,312.236818930251));
#16421=CARTESIAN_POINT('Ctrl Pts',(-36.2382361368719,1.58213284784921,312.231773612946));
#16422=CARTESIAN_POINT('Ctrl Pts',(-36.1868960372673,1.65994458793857,312.22672829564));
#16423=CARTESIAN_POINT('Ctrl Pts',(-36.1319136814722,1.7352238369019,312.221682978335));
#16424=CARTESIAN_POINT('Ctrl Pts',(-36.0769901674998,1.81042252241625,312.216643060501));
#16425=CARTESIAN_POINT('Ctrl Pts',(-36.0184324056657,1.88309374702584,312.211603142667));
#16426=CARTESIAN_POINT('Ctrl Pts',(-35.956505064021,1.95286980787962,312.206563224833));
#16427=CARTESIAN_POINT('Ctrl Pts',(-35.8946223616222,2.0225955718749,312.201526939936));
#16428=CARTESIAN_POINT('Ctrl Pts',(-35.8293752012407,2.08942998886531,312.196490655039));
#16429=CARTESIAN_POINT('Ctrl Pts',(-35.7610690412033,2.15303774065748,312.191454370142));
#16430=CARTESIAN_POINT('Ctrl Pts',(-35.6927877190443,2.21662236303343,312.186419916568));
#16431=CARTESIAN_POINT('Ctrl Pts',(-35.6214499317837,2.27698234864377,312.181385462994));
#16432=CARTESIAN_POINT('Ctrl Pts',(-35.54739783171,2.33381937989027,312.17635100942));
#16433=CARTESIAN_POINT('Ctrl Pts',(-35.4733519433136,2.3906516435029,312.171316978149));
#16434=CARTESIAN_POINT('Ctrl Pts',(-35.3965925473205,2.44396126995869,312.166282946877));
#16435=CARTESIAN_POINT('Ctrl Pts',(-35.3174937834037,2.49349109614537,312.161248915606));
#16436=CARTESIAN_POINT('Ctrl Pts',(-35.23837952742,2.54303062310796,312.156213898383));
#16437=CARTESIAN_POINT('Ctrl Pts',(-35.156925370263,2.58878864411495,312.15117888116));
#16438=CARTESIAN_POINT('Ctrl Pts',(-35.0735322551215,2.63055269103797,312.146143863937));
#16439=CARTESIAN_POINT('Ctrl Pts',(-34.9900475092246,2.67236262749475,312.141103314334));
#16440=CARTESIAN_POINT('Ctrl Pts',(-34.9046199504724,2.71016963065511,312.136062764731));
#16441=CARTESIAN_POINT('Ctrl Pts',(-34.8176725397979,2.74380850653966,312.131022215127));
#16442=CARTESIAN_POINT('Ctrl Pts',(-34.7306717107299,2.77746804933875,312.125978568732));
#16443=CARTESIAN_POINT('Ctrl Pts',(-34.6421495919806,2.80695422652558,312.120934922336));
#16444=CARTESIAN_POINT('Ctrl Pts',(-34.5525443253081,2.83215174102311,312.115891275941));
#16445=CARTESIAN_POINT('Ctrl Pts',(-34.4627939708205,2.8573900550457,312.110839462931));
#16446=CARTESIAN_POINT('Ctrl Pts',(-34.3719573994857,2.8783257435797,312.105787649922));
#16447=CARTESIAN_POINT('Ctrl Pts',(-34.2804827733287,2.89489465256765,312.100735836912));
#16448=CARTESIAN_POINT('Ctrl Pts',(-34.2341803714899,2.90328146226802,312.098178722597));
#16449=CARTESIAN_POINT('Ctrl Pts',(-34.1877145737566,2.91055026154907,312.095621608282));
#16450=CARTESIAN_POINT('Ctrl Pts',(-34.141143718015,2.91669781538954,312.093064493968));
#16451=CARTESIAN_POINT('Ctrl Pts',(-34.0491301834323,2.92884399885327,312.088012211318));
#16452=CARTESIAN_POINT('Ctrl Pts',(-33.9563761616878,2.9366535656255,312.082959928669));
#16453=CARTESIAN_POINT('Ctrl Pts',(-33.8633257974159,2.94004633011926,312.077907646019));
#16454=CARTESIAN_POINT('Ctrl Pts',(-33.7704037643636,2.94343441545235,312.072862331269));
#16455=CARTESIAN_POINT('Ctrl Pts',(-33.6771866410364,2.94241778698686,312.067817016519));
#16456=CARTESIAN_POINT('Ctrl Pts',(-33.5841258298458,2.93696775412617,312.06277170177));
#16457=CARTESIAN_POINT('Ctrl Pts',(-33.4911646101603,2.93152355376327,312.057731786398));
#16458=CARTESIAN_POINT('Ctrl Pts',(-33.3983598112263,2.9216554052996,312.052691871026));
#16459=CARTESIAN_POINT('Ctrl Pts',(-33.3061638809911,2.90738665622614,312.047651955654));
#16460=CARTESIAN_POINT('Ctrl Pts',(-33.2140344058603,2.89312819211002,312.042615673068));
#16461=CARTESIAN_POINT('Ctrl Pts',(-33.12251336487,2.87447549986094,312.037579390482));
#16462=CARTESIAN_POINT('Ctrl Pts',(-33.0320480735983,2.85150375622477,312.032543107897));
#16463=CARTESIAN_POINT('Ctrl Pts',(-32.9416156761503,2.82854036527806,312.027508656539));
#16464=CARTESIAN_POINT('Ctrl Pts',(-32.8522386959621,2.80126115201499,312.022474205181));
#16465=CARTESIAN_POINT('Ctrl Pts',(-32.7643532173439,2.76979217883517,312.017439753824));
#16466=CARTESIAN_POINT('Ctrl Pts',(-32.6764751090773,2.73832584474201,312.012405724671));
#16467=CARTESIAN_POINT('Ctrl Pts',(-32.590088671878,2.70267059926534,312.007371695518));
#16468=CARTESIAN_POINT('Ctrl Pts',(-32.5056127178106,2.66300168360263,312.002337666366));
#16469=CARTESIAN_POINT('Ctrl Pts',(-32.4211202168114,2.62332499769509,311.99730265116));
#16470=CARTESIAN_POINT('Ctrl Pts',(-32.3385393440913,2.57963326938745,311.992267635955));
#16471=CARTESIAN_POINT('Ctrl Pts',(-32.2582658556418,2.53214847837903,311.98723262075));
#16472=CARTESIAN_POINT('Ctrl Pts',(-32.1779041615258,2.48461151039763,311.982192072997));
#16473=CARTESIAN_POINT('Ctrl Pts',(-32.0998552955712,2.43327338668277,311.977151525245));
#16474=CARTESIAN_POINT('Ctrl Pts',(-32.0244871976255,2.3784001991587,311.972110977492));
#16475=CARTESIAN_POINT('Ctrl Pts',(-31.9490727939409,2.32349329785444,311.967067332855));
#16476=CARTESIAN_POINT('Ctrl Pts',(-31.8763427832563,2.26504728694481,311.962023688218));
#16477=CARTESIAN_POINT('Ctrl Pts',(-31.8066313816548,2.20336804360359,311.956980043581));
#16478=CARTESIAN_POINT('Ctrl Pts',(-31.7368071018819,2.14158892793105,311.951928232168));
#16479=CARTESIAN_POINT('Ctrl Pts',(-31.6700115070096,2.07656643765146,311.946876420755));
#16480=CARTESIAN_POINT('Ctrl Pts',(-31.6065412469252,2.00864257188561,311.941824609342));
#16481=CARTESIAN_POINT('Ctrl Pts',(-31.5744137457052,1.97426073577267,311.939267473495));
#16482=CARTESIAN_POINT('Ctrl Pts',(-31.543137612452,1.93913602706984,311.936710337647));
#16483=CARTESIAN_POINT('Ctrl Pts',(-31.51274716265,1.90331573629989,311.934153201799));
#16484=CARTESIAN_POINT('Ctrl Pts',(-31.4527031003815,1.83254364232026,311.929100929619));
#16485=CARTESIAN_POINT('Ctrl Pts',(-31.3959035223174,1.7588004031586,311.924048657439));
#16486=CARTESIAN_POINT('Ctrl Pts',(-31.3426563804786,1.6824159553422,311.918996385259));
#16487=CARTESIAN_POINT('Ctrl Pts',(-31.2894826771468,1.60613685702646,311.913951081178));
#16488=CARTESIAN_POINT('Ctrl Pts',(-31.2398519259153,1.52722414995996,311.908905777096));
#16489=CARTESIAN_POINT('Ctrl Pts',(-31.1940327208393,1.44604176124601,311.903860473014));
#16490=CARTESIAN_POINT('Ctrl Pts',(-31.1482625521689,1.36494625515107,311.898820568494));
#16491=CARTESIAN_POINT('Ctrl Pts',(-31.1062960388672,1.28158628031752,311.893780663973));
#16492=CARTESIAN_POINT('Ctrl Pts',(-31.0683585959412,1.19635482628272,311.888740759452));
#16493=CARTESIAN_POINT('Ctrl Pts',(-31.0304485002042,1.11118481130409,311.883704487944));
#16494=CARTESIAN_POINT('Ctrl Pts',(-30.9965618821709,1.02414640325922,311.878668216436));
#16495=CARTESIAN_POINT('Ctrl Pts',(-30.966877807416,0.93565634758182,311.873631944928));
#16496=CARTESIAN_POINT('Ctrl Pts',(-30.9372045268311,0.847198469989997,
311.868597504785));
#16497=CARTESIAN_POINT('Ctrl Pts',(-30.9117308947555,0.757290414202034,
311.863563064642));
#16498=CARTESIAN_POINT('Ctrl Pts',(-30.890587117435,0.66636704350975,311.858528624498));
#16499=CARTESIAN_POINT('Ctrl Pts',(-30.869445113818,0.575451300173184,311.853494606683));
#16500=CARTESIAN_POINT('Ctrl Pts',(-30.8526323432332,0.483520844028177,
311.848460588868));
#16501=CARTESIAN_POINT('Ctrl Pts',(-30.8402283156891,0.391022653483081,
311.843426571052));
#16502=CARTESIAN_POINT('Ctrl Pts',(-30.82782185874,0.298506346598925,311.838391567294));
#16503=CARTESIAN_POINT('Ctrl Pts',(-30.8198259183807,0.20542252482137,311.833356563535));
#16504=CARTESIAN_POINT('Ctrl Pts',(-30.8162682273124,0.112224097876667,
311.828321559776));
#16505=CARTESIAN_POINT('Ctrl Pts',(-30.8127066270613,0.0189232647127285,
311.823281023567));
#16506=CARTESIAN_POINT('Ctrl Pts',(-30.8135930276215,-0.074491980364185,
311.818240487358));
#16507=CARTESIAN_POINT('Ctrl Pts',(-30.8189030141255,-0.167568220223843,
311.813199951148));
#16508=CARTESIAN_POINT('Ctrl Pts',(-30.8242162629871,-0.260701644404563,
311.808156318127));
#16509=CARTESIAN_POINT('Ctrl Pts',(-30.8339584619861,-0.353495207224369,
311.803112685105));
#16510=CARTESIAN_POINT('Ctrl Pts',(-30.8480534866068,-0.445502293820143,
311.798069052083));
#16511=CARTESIAN_POINT('Ctrl Pts',(-30.8621713342437,-0.537658360590239,
311.793017252285));
#16512=CARTESIAN_POINT('Ctrl Pts',(-30.880655990392,-0.629024973895696,
311.787965452487));
#16513=CARTESIAN_POINT('Ctrl Pts',(-30.9033806193877,-0.719167535276973,
311.782913652689));
#16514=CARTESIAN_POINT('Ctrl Pts',(-30.9148839463684,-0.764798174995941,
311.780356405002));
#16515=CARTESIAN_POINT('Ctrl Pts',(-30.9274729521898,-0.810115424651446,
311.777799157316));
#16516=CARTESIAN_POINT('Ctrl Pts',(-30.9411264644474,-0.855064817799336,
311.77524190963));
#16517=CARTESIAN_POINT('Ctrl Pts',(-30.9681013021196,-0.943869995599242,
311.770189631511));
#16518=CARTESIAN_POINT('Ctrl Pts',(-30.999331001575,-1.03155685611456,311.765137353392));
#16519=CARTESIAN_POINT('Ctrl Pts',(-31.0347049864818,-1.11768783068693,
311.760085075273));
#16520=CARTESIAN_POINT('Ctrl Pts',(-31.0700301841841,-1.20370001486903,
311.755039765171));
#16521=CARTESIAN_POINT('Ctrl Pts',(-31.1094881421484,-1.28816016980654,
311.749994455069));
#16522=CARTESIAN_POINT('Ctrl Pts',(-31.1529183942683,-1.37064540401327,
311.744949144967));
#16523=CARTESIAN_POINT('Ctrl Pts',(-31.196302167356,-1.45304236256733,311.739909234353));
#16524=CARTESIAN_POINT('Ctrl Pts',(-31.2436495789414,-1.53346821042311,
311.73486932374));
#16525=CARTESIAN_POINT('Ctrl Pts',(-31.2947523465011,-1.61152061444348,
311.729829413126));
#16526=CARTESIAN_POINT('Ctrl Pts',(-31.3458182775324,-1.68951675576551,
311.724793135443));
#16527=CARTESIAN_POINT('Ctrl Pts',(-31.4006339413852,-1.76514248320502,
311.719756857759));
#16528=CARTESIAN_POINT('Ctrl Pts',(-31.4589459829763,-1.83802156107686,
311.714720580076));
#16529=CARTESIAN_POINT('Ctrl Pts',(-31.5172368208559,-1.91087413829977,
311.709686133709));
#16530=CARTESIAN_POINT('Ctrl Pts',(-31.5790212334917,-1.98098170354263,
311.704651687342));
#16531=CARTESIAN_POINT('Ctrl Pts',(-31.6440041734869,-2.04799928198917,
311.699617240975));
#16532=CARTESIAN_POINT('Ctrl Pts',(-31.7089816627469,-2.11501123903607,
311.694583216894));
#16533=CARTESIAN_POINT('Ctrl Pts',(-31.7771568365523,-2.17893340579648,
311.689549192814));
#16534=CARTESIAN_POINT('Ctrl Pts',(-31.848197006501,-2.23945686351124,311.684515168734));
#16535=CARTESIAN_POINT('Ctrl Pts',(-31.9192510905571,-2.2999921755035,311.679480158677));
#16536=CARTESIAN_POINT('Ctrl Pts',(-31.9931709468047,-2.35712716860007,
311.67444514862));
#16537=CARTESIAN_POINT('Ctrl Pts',(-32.0695908586993,-2.41059323795842,
311.669410138563));
#16538=CARTESIAN_POINT('Ctrl Pts',(-32.1460947406996,-2.46411805576835,
311.664369596043));
#16539=CARTESIAN_POINT('Ctrl Pts',(-32.2251037972259,-2.51396564760069,
311.659329053523));
#16540=CARTESIAN_POINT('Ctrl Pts',(-32.3062236426284,-2.55991097131137,
311.654288511003));
#16541=CARTESIAN_POINT('Ctrl Pts',(-32.3873933267648,-2.60588452309317,
311.649244871654));
#16542=CARTESIAN_POINT('Ctrl Pts',(-32.470675985273,-2.64795083367218,311.644201232306));
#16543=CARTESIAN_POINT('Ctrl Pts',(-32.5556549453796,-2.68593201429846,
311.639157592957));
#16544=CARTESIAN_POINT('Ctrl Pts',(-32.6407715047558,-2.7239746946502,311.634105786868));
#16545=CARTESIAN_POINT('Ctrl Pts',(-32.7275894358986,-2.75791887803125,
311.62905398078));
#16546=CARTESIAN_POINT('Ctrl Pts',(-32.815674702911,-2.78763581362287,311.624002174691));
#16547=CARTESIAN_POINT('Ctrl Pts',(-32.8602627937985,-2.80267829995457,
311.621444988947));
#16548=CARTESIAN_POINT('Ctrl Pts',(-32.9051754117061,-2.81663844162384,
311.618887803204));
#16549=CARTESIAN_POINT('Ctrl Pts',(-32.95035530731,-2.82950453941247,311.61633061746));
#16550=CARTESIAN_POINT('Ctrl Pts',(-33.0396180316545,-2.85492431794327,
311.611278340046));
#16551=CARTESIAN_POINT('Ctrl Pts',(-33.1302450405338,-2.87616160923921,
311.606226062632));
#16552=CARTESIAN_POINT('Ctrl Pts',(-33.2218086080801,-2.89307238572852,
311.601173785217));
#16553=CARTESIAN_POINT('Ctrl Pts',(-33.3132458927251,-2.90995983916505,
311.596128475818));
#16554=CARTESIAN_POINT('Ctrl Pts',(-33.4056167362174,-2.92253255510562,
311.591083166418));
#16555=CARTESIAN_POINT('Ctrl Pts',(-33.4984787311459,-2.9306963944669,311.586037857018));
#16556=CARTESIAN_POINT('Ctrl Pts',(-33.5912413452703,-2.93885149689636,
311.580997947103));
#16557=CARTESIAN_POINT('Ctrl Pts',(-33.684493625891,-2.94260706253087,311.575958037187));
#16558=CARTESIAN_POINT('Ctrl Pts',(-33.7777845509332,-2.94192028300932,
311.570918127272));
#16559=CARTESIAN_POINT('Ctrl Pts',(-33.8710082290045,-2.94123399853959,
311.565881850279));
#16560=CARTESIAN_POINT('Ctrl Pts',(-33.9642700531627,-2.93611173695307,
311.560845573286));
#16561=CARTESIAN_POINT('Ctrl Pts',(-34.0571165291237,-2.92656271392951,
311.555809296293));
#16562=CARTESIAN_POINT('Ctrl Pts',(-34.1499292438889,-2.91701716315874,
311.55077485061));
#16563=CARTESIAN_POINT('Ctrl Pts',(-34.2423264690152,-2.90304809414868,
311.545740404928));
#16564=CARTESIAN_POINT('Ctrl Pts',(-34.3338584093083,-2.88471670149476,
311.540705959245));
#16565=CARTESIAN_POINT('Ctrl Pts',(-34.425382672065,-2.86638684644549,311.535671935843));
#16566=CARTESIAN_POINT('Ctrl Pts',(-34.5160413587211,-2.84369548267463,
311.530637912441));
#16567=CARTESIAN_POINT('Ctrl Pts',(-34.6053945983624,-2.81675497501515,
311.525603889039));
#16568=CARTESIAN_POINT('Ctrl Pts',(-34.6947653390869,-2.78980919068004,
311.520568879653));
#16569=CARTESIAN_POINT('Ctrl Pts',(-34.7828296997837,-2.75861273818651,
311.515533870266));
#16570=CARTESIAN_POINT('Ctrl Pts',(-34.8691638114394,-2.72332758084775,
311.51049886088));
#16571=CARTESIAN_POINT('Ctrl Pts',(-34.9555927871857,-2.68800365210917,
311.505458319016));
#16572=CARTESIAN_POINT('Ctrl Pts',(-35.0402873069962,-2.64858221894387,
311.500417777152));
#16573=CARTESIAN_POINT('Ctrl Pts',(-35.1228445956338,-2.60527293825904,
311.495377235287));
#16574=CARTESIAN_POINT('Ctrl Pts',(-35.2054526062804,-2.56193704897603,
311.490333596587));
#16575=CARTESIAN_POINT('Ctrl Pts',(-35.2859203888052,-2.51470878157065,
311.485289957886));
#16576=CARTESIAN_POINT('Ctrl Pts',(-35.3638727366605,-2.46384206625863,
311.480246319186));
#16577=CARTESIAN_POINT('Ctrl Pts',(-35.4419513064852,-2.41289298656428,
311.475194513727));
#16578=CARTESIAN_POINT('Ctrl Pts',(-35.5175059506873,-2.3582939572961,311.470142708267));
#16579=CARTESIAN_POINT('Ctrl Pts',(-35.5901933664827,-2.3003401174577,311.465090902808));
#16580=CARTESIAN_POINT('Ctrl Pts',(-35.6269872843073,-2.27100424415282,
311.462533710302));
#16581=CARTESIAN_POINT('Ctrl Pts',(-35.6630470935547,-2.24080936808293,
311.459976517797));
#16582=CARTESIAN_POINT('Ctrl Pts',(-35.6983319533873,-2.20979727965005,
311.457419325291));
#16583=CARTESIAN_POINT('Ctrl Pts',(-35.7670192133601,-2.14942760861852,
311.4524413674));
#16584=CARTESIAN_POINT('Ctrl Pts',(-35.8330298232882,-2.08572835462146,
311.447463409509));
#16585=CARTESIAN_POINT('Ctrl Pts',(-35.8960161596962,-2.01896966106762,
311.442485451618));
#16586=CARTESIAN_POINT('Ctrl Pts',(-35.959444480282,-1.95174251216369,311.43747256268));
#16587=CARTESIAN_POINT('Ctrl Pts',(-36.0198055125062,-1.88141306145673,
311.432459673743));
#16588=CARTESIAN_POINT('Ctrl Pts',(-36.0767772751384,-1.80829931640985,
311.427446784806));
#16589=CARTESIAN_POINT('Ctrl Pts',(-36.1332079540307,-1.73587996200101,
311.42248150529));
#16590=CARTESIAN_POINT('Ctrl Pts',(-36.1863131607934,-1.66072932853249,
311.417516225775));
#16591=CARTESIAN_POINT('Ctrl Pts',(-36.2358173502925,-1.58319294210419,
311.41255094626));
#16592=CARTESIAN_POINT('Ctrl Pts',(-36.2852909788572,-1.50570442201681,
311.407588732012));
#16593=CARTESIAN_POINT('Ctrl Pts',(-36.3311677570923,-1.42583345800156,
311.402626517764));
#16594=CARTESIAN_POINT('Ctrl Pts',(-36.3732143473538,-1.34395608132238,
311.397664303517));
#16595=CARTESIAN_POINT('Ctrl Pts',(-36.4152475509804,-1.26210477245377,
311.39270366912));
#16596=CARTESIAN_POINT('Ctrl Pts',(-36.4534527797942,-1.17824872743093,
311.387743034723));
#16597=CARTESIAN_POINT('Ctrl Pts',(-36.487642382713,-1.0927890244623,311.382782400327));
#16598=CARTESIAN_POINT('Ctrl Pts',(-36.5224515185249,-1.00578074846246,
311.377731876726));
#16599=CARTESIAN_POINT('Ctrl Pts',(-36.5530978472644,-0.917110563339265,
311.372681353126));
#16600=CARTESIAN_POINT('Ctrl Pts',(-36.5794349219442,-0.8272221711891,311.367630829525));
#16601=CARTESIAN_POINT('Ctrl Pts',(-36.6053216305679,-0.738870877640935,
311.362666670277));
#16602=CARTESIAN_POINT('Ctrl Pts',(-36.6270452419933,-0.649343179726609,
311.357702511029));
#16603=CARTESIAN_POINT('Ctrl Pts',(-36.6445177946938,-0.55907312852248,
311.352738351781));
#16604=CARTESIAN_POINT('Ctrl Pts',(-36.662446317566,-0.466447356808736,
311.347644646005));
#16605=CARTESIAN_POINT('Ctrl Pts',(-36.67589872875,-0.373040454094561,311.342550940228));
#16606=CARTESIAN_POINT('Ctrl Pts',(-36.6848366520725,-0.279327624487683,
311.337457234452));
#16607=CARTESIAN_POINT('Ctrl Pts',(-36.6937745753949,-0.185614794880804,
311.332363528675));
#16608=CARTESIAN_POINT('Ctrl Pts',(-36.6981980415015,-0.0915965565959887,
311.327269822898));
#16609=CARTESIAN_POINT('Ctrl Pts',(-36.6981261623761,0.00225326298871554,
311.322176117122));
#16610=CARTESIAN_POINT('',(-36.6981262001274,-0.00220342124124626,310.322176117056));
#16611=CARTESIAN_POINT('Ctrl Pts',(-36.6981261623756,0.00225326359443262,
311.322176117089));
#16612=CARTESIAN_POINT('Ctrl Pts',(-36.6980148327132,0.1476120984491,311.314286755767));
#16613=CARTESIAN_POINT('Ctrl Pts',(-36.6871291095033,0.29256686069583,311.306397394444));
#16614=CARTESIAN_POINT('Ctrl Pts',(-36.6656558427427,0.435896845852016,
311.298508033121));
#16615=CARTESIAN_POINT('Ctrl Pts',(-36.6519045529365,0.527684098614721,
311.29345575602));
#16616=CARTESIAN_POINT('Ctrl Pts',(-36.633780885816,0.618984748458059,311.288403478919));
#16617=CARTESIAN_POINT('Ctrl Pts',(-36.6113304995924,0.709349786879677,
311.283351201818));
#16618=CARTESIAN_POINT('Ctrl Pts',(-36.5889110766032,0.799590195202268,
311.278305892742));
#16619=CARTESIAN_POINT('Ctrl Pts',(-36.5621768985692,0.888897128846525,
311.273260583666));
#16620=CARTESIAN_POINT('Ctrl Pts',(-36.5312251193052,0.976828832709801,
311.268215274589));
#16621=CARTESIAN_POINT('Ctrl Pts',(-36.500306464662,1.06466643198808,311.263175365007));
#16622=CARTESIAN_POINT('Ctrl Pts',(-36.4651793271225,1.15113131005255,311.258135455425));
#16623=CARTESIAN_POINT('Ctrl Pts',(-36.4259911615463,1.23579508566736,311.253095545842));
#16624=CARTESIAN_POINT('Ctrl Pts',(-36.3868312441088,1.32039783280476,311.248059269195));
#16625=CARTESIAN_POINT('Ctrl Pts',(-36.3436163031757,1.40320165603155,311.243022992548));
#16626=CARTESIAN_POINT('Ctrl Pts',(-36.2965421869159,1.48379742768906,311.237986715901));
#16627=CARTESIAN_POINT('Ctrl Pts',(-36.2494851880039,1.56436389267091,311.232952270573));
#16628=CARTESIAN_POINT('Ctrl Pts',(-36.1985720253936,1.64272351790864,311.227917825244));
#16629=CARTESIAN_POINT('Ctrl Pts',(-36.1440443485017,1.71849203005162,311.222883379916));
#16630=CARTESIAN_POINT('Ctrl Pts',(-36.0895212453757,1.79425418675342,311.217849356875));
#16631=CARTESIAN_POINT('Ctrl Pts',(-36.0313844904188,1.86742530200637,311.212815333834));
#16632=CARTESIAN_POINT('Ctrl Pts',(-35.9699182246906,1.93765129094818,311.207781310794));
#16633=CARTESIAN_POINT('Ctrl Pts',(-35.908439920019,2.00789103453554,311.202746301776));
#16634=CARTESIAN_POINT('Ctrl Pts',(-35.8436311023061,2.07518417217566,311.197711292758));
#16635=CARTESIAN_POINT('Ctrl Pts',(-35.7758144608132,2.13921169187599,311.192676283741));
#16636=CARTESIAN_POINT('Ctrl Pts',(-35.7079233023717,2.20330956503658,311.187635742254));
#16637=CARTESIAN_POINT('Ctrl Pts',(-35.6370180465144,2.26413435220616,311.182595200767));
#16638=CARTESIAN_POINT('Ctrl Pts',(-35.5634560913953,2.32140596335365,311.177554659279));
#16639=CARTESIAN_POINT('Ctrl Pts',(-35.4898489409464,2.37871276129504,311.172511020961));
#16640=CARTESIAN_POINT('Ctrl Pts',(-35.4135822046436,2.43246178152501,311.167467382643));
#16641=CARTESIAN_POINT('Ctrl Pts',(-35.3350421986589,2.48241633800681,311.162423744325));
#16642=CARTESIAN_POINT('Ctrl Pts',(-35.2563750192213,2.53245178184475,311.157371939253));
#16643=CARTESIAN_POINT('Ctrl Pts',(-35.1754276068903,2.57868027601982,311.152320134181));
#16644=CARTESIAN_POINT('Ctrl Pts',(-35.0926106134532,2.62091121911518,311.147268329109));
#16645=CARTESIAN_POINT('Ctrl Pts',(-35.0506891050683,2.64228829115798,311.144711133057));
#16646=CARTESIAN_POINT('Ctrl Pts',(-35.0082888671287,2.66264182700462,311.142153937005));
#16647=CARTESIAN_POINT('Ctrl Pts',(-34.965464834845,2.68195191274982,311.139596740952));
#16648=CARTESIAN_POINT('Ctrl Pts',(-34.8808569799058,2.72010303599686,311.134544463969));
#16649=CARTESIAN_POINT('Ctrl Pts',(-34.7942901489513,2.75431501252286,311.129492186985));
#16650=CARTESIAN_POINT('Ctrl Pts',(-34.7061665257702,2.78438304611017,311.124439910002));
#16651=CARTESIAN_POINT('Ctrl Pts',(-34.6181644413726,2.8144096103151,311.119394601043));
#16652=CARTESIAN_POINT('Ctrl Pts',(-34.5286102481237,2.84030344632051,311.114349292085));
#16653=CARTESIAN_POINT('Ctrl Pts',(-34.437927921793,2.86190697568658,311.109303983126));
#16654=CARTESIAN_POINT('Ctrl Pts',(-34.3473426437734,2.88348738493516,311.104264073662));
#16655=CARTESIAN_POINT('Ctrl Pts',(-34.2556320622605,2.90078651142138,311.099224164198));
#16656=CARTESIAN_POINT('Ctrl Pts',(-34.1632361529169,2.91369630506964,311.094184254733));
#16657=CARTESIAN_POINT('Ctrl Pts',(-34.0709068456309,2.92659679290744,311.089147978204));
#16658=CARTESIAN_POINT('Ctrl Pts',(-33.9778936311397,2.93511417545618,311.084111701675));
#16659=CARTESIAN_POINT('Ctrl Pts',(-33.8846465090519,2.93919151167209,311.079075425146));
#16660=CARTESIAN_POINT('Ctrl Pts',(-33.7914332939919,2.94326736526473,311.074040979935));
#16661=CARTESIAN_POINT('Ctrl Pts',(-33.6979867836906,2.94290636054035,311.069006534724));
#16662=CARTESIAN_POINT('Ctrl Pts',(-33.6047608896535,2.93810351978828,311.063972089513));
#16663=CARTESIAN_POINT('Ctrl Pts',(-33.5115428153734,2.9333010818969,311.05893806659));
#16664=CARTESIAN_POINT('Ctrl Pts',(-33.4185457642236,2.92405757179316,311.053904043667));
#16665=CARTESIAN_POINT('Ctrl Pts',(-33.326221283017,2.9104200818419,311.048870020744));
#16666=CARTESIAN_POINT('Ctrl Pts',(-33.2338787188888,2.8967799208151,311.043835011843));
#16667=CARTESIAN_POINT('Ctrl Pts',(-33.1422094257301,2.87874413603304,311.038800002943));
#16668=CARTESIAN_POINT('Ctrl Pts',(-33.0516563439135,2.85641122024238,311.033764994042));
#16669=CARTESIAN_POINT('Ctrl Pts',(-32.9610037623138,2.83405376502985,311.028724452671));
#16670=CARTESIAN_POINT('Ctrl Pts',(-32.8714702722827,2.80738986029844,311.023683911299));
#16671=CARTESIAN_POINT('Ctrl Pts',(-32.7834848927091,2.77656825631777,311.018643369928));
#16672=CARTESIAN_POINT('Ctrl Pts',(-32.6954454562649,2.74572771601533,311.013599731725));
#16673=CARTESIAN_POINT('Ctrl Pts',(-32.6089564353067,2.71072455764135,311.008556093522));
#16674=CARTESIAN_POINT('Ctrl Pts',(-32.5244260231715,2.67175534835436,311.003512455319));
#16675=CARTESIAN_POINT('Ctrl Pts',(-32.4397587377679,2.63272303937452,310.99846065036));
#16676=CARTESIAN_POINT('Ctrl Pts',(-32.3570567861788,2.58971206365978,310.993408845401));
#16677=CARTESIAN_POINT('Ctrl Pts',(-32.2767028009575,2.54296440489324,310.988357040442));
#16678=CARTESIAN_POINT('Ctrl Pts',(-32.2360280343565,2.51930098478736,310.985799843223));
#16679=CARTESIAN_POINT('Ctrl Pts',(-32.195954421594,2.49468078637952,310.983242646003));
#16680=CARTESIAN_POINT('Ctrl Pts',(-32.1565284555702,2.46913920544266,310.980685448783));
#16681=CARTESIAN_POINT('Ctrl Pts',(-32.0786342298843,2.41867648073303,310.975633171884));
#16682=CARTESIAN_POINT('Ctrl Pts',(-32.0029904579736,2.36443355494242,310.970580894984));
#16683=CARTESIAN_POINT('Ctrl Pts',(-31.9299871189817,2.30663760541324,310.965528618085));
#16684=CARTESIAN_POINT('Ctrl Pts',(-31.8570844651319,2.2489213672161,310.960483309213));
#16685=CARTESIAN_POINT('Ctrl Pts',(-31.7868153530777,2.18766211611815,310.95543800034));
#16686=CARTESIAN_POINT('Ctrl Pts',(-31.719541870994,2.12313092140667,310.950392691468));
#16687=CARTESIAN_POINT('Ctrl Pts',(-31.6523403850784,2.05866878806375,310.945352782092));
#16688=CARTESIAN_POINT('Ctrl Pts',(-31.5881284757504,1.99094197702334,310.940312872715));
#16689=CARTESIAN_POINT('Ctrl Pts',(-31.5272352609016,1.92026183183079,310.935272963339));
#16690=CARTESIAN_POINT('Ctrl Pts',(-31.4663859399434,1.84963263527946,310.9302366869));
#16691=CARTESIAN_POINT('Ctrl Pts',(-31.4088508477137,1.77605467159468,310.925200410461));
#16692=CARTESIAN_POINT('Ctrl Pts',(-31.3549215665312,1.69987539101623,310.920164134022));
#16693=CARTESIAN_POINT('Ctrl Pts',(-31.3010118954231,1.62372381118455,310.915129688903));
#16694=CARTESIAN_POINT('Ctrl Pts',(-31.2507056870232,1.54497315582983,310.910095243784));
#16695=CARTESIAN_POINT('Ctrl Pts',(-31.2042529596907,1.46400230651697,310.905060798664));
#16696=CARTESIAN_POINT('Ctrl Pts',(-31.1578041288089,1.38303824903183,310.900026775834));
#16697=CARTESIAN_POINT('Ctrl Pts',(-31.1152083572513,1.29985475329337,310.894992753003));
#16698=CARTESIAN_POINT('Ctrl Pts',(-31.076670610348,1.21485691363216,310.889958730173));
#16699=CARTESIAN_POINT('Ctrl Pts',(-31.0381253153461,1.12984242608344,310.884923721366));
#16700=CARTESIAN_POINT('Ctrl Pts',(-31.0036398066047,1.04301329360174,310.87988871256));
#16701=CARTESIAN_POINT('Ctrl Pts',(-30.9733711789297,0.954795213502898,
310.874853703753));
#16702=CARTESIAN_POINT('Ctrl Pts',(-30.9430692920738,0.866480199340128,
310.869813162476));
#16703=CARTESIAN_POINT('Ctrl Pts',(-30.9169936797229,0.776773611991706,
310.8647726212));
#16704=CARTESIAN_POINT('Ctrl Pts',(-30.8952516483215,0.686116664745062,
310.859732079923));
#16705=CARTESIAN_POINT('Ctrl Pts',(-30.8734962589519,0.595404019270442,
310.854688441816));
#16706=CARTESIAN_POINT('Ctrl Pts',(-30.8560798338832,0.503740287619101,
310.849644803709));
#16707=CARTESIAN_POINT('Ctrl Pts',(-30.843058203726,0.41157507337135,310.844601165602));
#16708=CARTESIAN_POINT('Ctrl Pts',(-30.8300154886953,0.319260623439119,
310.839549360739));
#16709=CARTESIAN_POINT('Ctrl Pts',(-30.8213818161632,0.226443511624768,
310.834497555876));
#16710=CARTESIAN_POINT('Ctrl Pts',(-30.8171609942021,0.133576451149687,
310.829445751013));
#16711=CARTESIAN_POINT('Ctrl Pts',(-30.8150244354211,0.0865676136897683,
310.82688855288));
#16712=CARTESIAN_POINT('Ctrl Pts',(-30.8140177651276,0.0395459504315597,
310.824331354747));
#16713=CARTESIAN_POINT('Ctrl Pts',(-30.8141364081974,-0.00743028464432902,
310.821774156614));
#16714=CARTESIAN_POINT('Ctrl Pts',(-30.814370812267,-0.100241611016934,
310.816721879646));
#16715=CARTESIAN_POINT('Ctrl Pts',(-30.8190018384742,-0.19320842813451,
310.811669602677));
#16716=CARTESIAN_POINT('Ctrl Pts',(-30.8280497205578,-0.285879865856423,
310.806617325709));
#16717=CARTESIAN_POINT('Ctrl Pts',(-30.8370851239363,-0.378423492501761,
310.801572016766));
#16718=CARTESIAN_POINT('Ctrl Pts',(-30.850525235491,-0.470672110956442,
310.796526707824));
#16719=CARTESIAN_POINT('Ctrl Pts',(-30.8683382860445,-0.562174525991569,
310.791481398881));
#16720=CARTESIAN_POINT('Ctrl Pts',(-30.8861322730517,-0.653579015041502,
310.786441489434));
#16721=CARTESIAN_POINT('Ctrl Pts',(-30.9082898125679,-0.74423845425817,
310.781401579986));
#16722=CARTESIAN_POINT('Ctrl Pts',(-30.934727422777,-0.833707552516224,
310.776361670539));
#16723=CARTESIAN_POINT('Ctrl Pts',(-30.9611459758679,-0.923112158440201,
310.771325394027));
#16724=CARTESIAN_POINT('Ctrl Pts',(-30.9918383418163,-1.01132770405547,
310.766289117516));
#16725=CARTESIAN_POINT('Ctrl Pts',(-31.0266703570855,-1.09792089722844,
310.761252841005));
#16726=CARTESIAN_POINT('Ctrl Pts',(-31.0614897065423,-1.1844826028998,310.756218395812));
#16727=CARTESIAN_POINT('Ctrl Pts',(-31.1004455492921,-1.26942271633927,
310.75118395062));
#16728=CARTESIAN_POINT('Ctrl Pts',(-31.1433547886595,-1.35232586297179,
310.746149505428));
#16729=CARTESIAN_POINT('Ctrl Pts',(-31.1862604288087,-1.43522205570513,
310.741115482524));
#16730=CARTESIAN_POINT('Ctrl Pts',(-31.2331186018868,-1.5160812268844,310.73608145962));
#16731=CARTESIAN_POINT('Ctrl Pts',(-31.2836997753803,-1.59451167887353,
310.731047436716));
#16732=CARTESIAN_POINT('Ctrl Pts',(-31.3342908558324,-1.67295749245256,
310.726012427835));
#16733=CARTESIAN_POINT('Ctrl Pts',(-31.3886061438107,-1.7489732689834,310.720977418954));
#16734=CARTESIAN_POINT('Ctrl Pts',(-31.4463728608584,-1.82219639447585,
310.715942410074));
#16735=CARTESIAN_POINT('Ctrl Pts',(-31.5042030520017,-1.89549997757259,
310.710901868723));
#16736=CARTESIAN_POINT('Ctrl Pts',(-31.5654919667713,-1.96600443508492,
310.705861327372));
#16737=CARTESIAN_POINT('Ctrl Pts',(-31.6299268184473,-2.03338060395983,
310.700820786021));
#16738=CARTESIAN_POINT('Ctrl Pts',(-31.6944012579037,-2.10079816771507,
310.695777147839));
#16739=CARTESIAN_POINT('Ctrl Pts',(-31.7620251603763,-2.16508331070172,
310.690733509658));
#16740=CARTESIAN_POINT('Ctrl Pts',(-31.8324508071149,-2.22594559856081,
310.685689871476));
#16741=CARTESIAN_POINT('Ctrl Pts',(-31.9029904884068,-2.28690643579974,
310.680638066539));
#16742=CARTESIAN_POINT('Ctrl Pts',(-31.9763406216714,-2.34443307946837,
310.675586261602));
#16743=CARTESIAN_POINT('Ctrl Pts',(-32.0521226991807,-2.39827714343257,
310.670534456665));
#16744=CARTESIAN_POINT('Ctrl Pts',(-32.0904831930016,-2.42553272880159,
310.667977259258));
#16745=CARTESIAN_POINT('Ctrl Pts',(-32.1294664045489,-2.45184542834957,
310.665420061851));
#16746=CARTESIAN_POINT('Ctrl Pts',(-32.1690208852344,-2.4771875383791,310.662862864445));
#16747=CARTESIAN_POINT('Ctrl Pts',(-32.2471690135683,-2.52725616353908,
310.657810587493));
#16748=CARTESIAN_POINT('Ctrl Pts',(-32.3278290201464,-2.57371301198809,
310.652758310541));
#16749=CARTESIAN_POINT('Ctrl Pts',(-32.4106328426013,-2.61629688767119,
310.647706033589));
#16750=CARTESIAN_POINT('Ctrl Pts',(-32.4933224632462,-2.6588220323014,310.642660724663));
#16751=CARTESIAN_POINT('Ctrl Pts',(-32.578149632747,-2.69748461708396,310.637615415737));
#16752=CARTESIAN_POINT('Ctrl Pts',(-32.6647178511997,-2.73206698577875,
310.632570106811));
#16753=CARTESIAN_POINT('Ctrl Pts',(-32.7511934242478,-2.76661234438375,
310.627530197381));
#16754=CARTESIAN_POINT('Ctrl Pts',(-32.8394059323737,-2.79708600235729,
310.62249028795));
#16755=CARTESIAN_POINT('Ctrl Pts',(-32.9289358318737,-2.82331697292177,
310.617450378519));
#16756=CARTESIAN_POINT('Ctrl Pts',(-33.0184011952104,-2.84952903532029,
310.612414102025));
#16757=CARTESIAN_POINT('Ctrl Pts',(-33.10918163731,-2.87150436450134,310.60737782553));
#16758=CARTESIAN_POINT('Ctrl Pts',(-33.2008402526277,-2.88912107744592,
310.602341549036));
#16759=CARTESIAN_POINT('Ctrl Pts',(-33.2924655385258,-2.90673138450256,
310.59730710386));
#16760=CARTESIAN_POINT('Ctrl Pts',(-33.3849679274346,-2.91998614013725,
310.592272658685));
#16761=CARTESIAN_POINT('Ctrl Pts',(-33.4778990743842,-2.9288143005921,310.58723821351));
#16762=CARTESIAN_POINT('Ctrl Pts',(-33.5708224262876,-2.9376417205426,310.582204190623));
#16763=CARTESIAN_POINT('Ctrl Pts',(-33.6641740224438,-2.94204324171661,
310.577170167736));
#16764=CARTESIAN_POINT('Ctrl Pts',(-33.7575002725516,-2.94199967950234,
310.572136144848));
#16765=CARTESIAN_POINT('Ctrl Pts',(-33.8508448017788,-2.94195610875586,
310.567101135985));
#16766=CARTESIAN_POINT('Ctrl Pts',(-33.9441635308687,-2.93746572613335,
310.562066127121));
#16767=CARTESIAN_POINT('Ctrl Pts',(-34.0370038969137,-2.92856145282435,
310.557031118257));
#16768=CARTESIAN_POINT('Ctrl Pts',(-34.1299462759984,-2.91964739549548,
310.551990576923));
#16769=CARTESIAN_POINT('Ctrl Pts',(-34.2224087999158,-2.90630980881408,
310.546950035589));
#16770=CARTESIAN_POINT('Ctrl Pts',(-34.3139453579785,-2.88863336331914,
310.541909494255));
#16771=CARTESIAN_POINT('Ctrl Pts',(-34.4055381546934,-2.87094605768821,
310.53686585609));
#16772=CARTESIAN_POINT('Ctrl Pts',(-34.4962034216126,-2.84891469112421,
310.531822217925));
#16773=CARTESIAN_POINT('Ctrl Pts',(-34.5855086862144,-2.82267427459644,
310.52677857976));
#16774=CARTESIAN_POINT('Ctrl Pts',(-34.674958555612,-2.79639136908337,310.52172677484));
#16775=CARTESIAN_POINT('Ctrl Pts',(-34.7630436071173,-2.76588595274888,
310.516674969919));
#16776=CARTESIAN_POINT('Ctrl Pts',(-34.8493500407492,-2.7313416919894,310.511623164999));
#16777=CARTESIAN_POINT('Ctrl Pts',(-34.8930379119615,-2.71385556550174,
310.509065967424));
#16778=CARTESIAN_POINT('Ctrl Pts',(-34.9362704105143,-2.69533529825263,
310.50650876985));
#16779=CARTESIAN_POINT('Ctrl Pts',(-34.9789963834475,-2.67580913609329,
310.503951572275));
#16780=CARTESIAN_POINT('Ctrl Pts',(-35.0634104506821,-2.63723113184438,
310.49889929533));
#16781=CARTESIAN_POINT('Ctrl Pts',(-35.1461487115125,-2.59458543339695,
310.493847018385));
#16782=CARTESIAN_POINT('Ctrl Pts',(-35.2267922544889,-2.54803998860497,
310.48879474144));
#16783=CARTESIAN_POINT('Ctrl Pts',(-35.3073245750781,-2.5015587386052,310.483749432521));
#16784=CARTESIAN_POINT('Ctrl Pts',(-35.3857675372035,-2.45118865011851,
310.478704123603));
#16785=CARTESIAN_POINT('Ctrl Pts',(-35.4617234293671,-2.39714515753402,
310.473658814684));
#16786=CARTESIAN_POINT('Ctrl Pts',(-35.5375980334471,-2.34315950235777,
310.46861890526));
#16787=CARTESIAN_POINT('Ctrl Pts',(-35.6109904979903,-2.28550851326761,
310.463578995837));
#16788=CARTESIAN_POINT('Ctrl Pts',(-35.6815298635595,-2.22445227196699,
310.458539086413));
#16789=CARTESIAN_POINT('Ctrl Pts',(-35.7520183819782,-2.16344004206148,
310.453502809926));
#16790=CARTESIAN_POINT('Ctrl Pts',(-35.8196575542849,-2.09902772875571,
310.44846653344));
#16791=CARTESIAN_POINT('Ctrl Pts',(-35.8841082967683,-2.03151660295942,
310.443430256953));
#16792=CARTESIAN_POINT('Ctrl Pts',(-35.9485356033097,-1.96403002593893,
310.438395811785));
#16793=CARTESIAN_POINT('Ctrl Pts',(-36.0097764768289,-1.89344719596275,
310.433361366617));
#16794=CARTESIAN_POINT('Ctrl Pts',(-36.0675283757988,-1.82010653444136,
310.428326921449));
#16795=CARTESIAN_POINT('Ctrl Pts',(-36.1252754305495,-1.74677202472187,
310.42329289857));
#16796=CARTESIAN_POINT('Ctrl Pts',(-36.1795338179152,-1.67068049253444,
310.418258875691));
#16797=CARTESIAN_POINT('Ctrl Pts',(-36.2300417505706,-1.59220285512856,
310.413224852811));
#16798=CARTESIAN_POINT('Ctrl Pts',(-36.2805595758385,-1.51370984689249,
310.408189843955));
#16799=CARTESIAN_POINT('Ctrl Pts',(-36.3273252474256,-1.43283017903317,
310.403154835099));
#16800=CARTESIAN_POINT('Ctrl Pts',(-36.3701213368016,-1.34996212510415,
310.398119826244));
#16801=CARTESIAN_POINT('Ctrl Pts',(-36.4129644505407,-1.26700301571866,
310.393079284918));
#16802=CARTESIAN_POINT('Ctrl Pts',(-36.4518290712748,-1.18205155440164,
310.388038743592));
#16803=CARTESIAN_POINT('Ctrl Pts',(-36.4865447676517,-1.09552861761781,
310.382998202266));
#16804=CARTESIAN_POINT('Ctrl Pts',(-36.5212817928175,-1.00895252247476,
310.377954564109));
#16805=CARTESIAN_POINT('Ctrl Pts',(-36.551864673487,-0.920803449165568,
310.372910925952));
#16806=CARTESIAN_POINT('Ctrl Pts',(-36.5781726829229,-0.831518073196525,
310.367867287795));
#16807=CARTESIAN_POINT('Ctrl Pts',(-36.6045232907916,-0.742088124636358,
310.362815482882));
#16808=CARTESIAN_POINT('Ctrl Pts',(-36.6265851035865,-0.651518631330701,
310.35776367797));
#16809=CARTESIAN_POINT('Ctrl Pts',(-36.6442884092663,-0.560256923135343,
310.352711873057));
#16810=CARTESIAN_POINT('Ctrl Pts',(-36.6532497315015,-0.514060716072903,
310.350154675407));
#16811=CARTESIAN_POINT('Ctrl Pts',(-36.6610950854093,-0.467687234593608,
310.347597477756));
#16812=CARTESIAN_POINT('Ctrl Pts',(-36.6678205117366,-0.421194777740095,
310.345040280106));
#16813=CARTESIAN_POINT('Ctrl Pts',(-36.6878647509024,-0.282630190273806,
310.337418892434));
#16814=CARTESIAN_POINT('Ctrl Pts',(-36.6980210483658,-0.14260159061453,
310.329797504762));
#16815=CARTESIAN_POINT('Ctrl Pts',(-36.698126200127,-0.00220342186298763,
310.32217611709));
#16816=CARTESIAN_POINT('',(-36.6981268542406,-0.00100312718013536,309.322176117137));
#16817=CARTESIAN_POINT('Ctrl Pts',(-36.6981262001274,-0.00220342124124822,
310.322176117056));
#16818=CARTESIAN_POINT('Ctrl Pts',(-36.6981948132346,0.0894085233407486,
310.317203045461));
#16819=CARTESIAN_POINT('Ctrl Pts',(-36.6939801246682,0.181182574134905,
310.312229973866));
#16820=CARTESIAN_POINT('Ctrl Pts',(-36.6854632440038,0.272678047413998,
310.30725690227));
#16821=CARTESIAN_POINT('Ctrl Pts',(-36.6768197596925,0.365533603222195,
310.30220990584));
#16822=CARTESIAN_POINT('Ctrl Pts',(-36.6637450630147,0.458101758252811,
310.297162909409));
#16823=CARTESIAN_POINT('Ctrl Pts',(-36.6462743635366,0.549920324264078,
310.292115912979));
#16824=CARTESIAN_POINT('Ctrl Pts',(-36.6290924162591,0.640221331518039,
310.287152332288));
#16825=CARTESIAN_POINT('Ctrl Pts',(-36.6076587613469,0.729796870639183,
310.282188751598));
#16826=CARTESIAN_POINT('Ctrl Pts',(-36.5820590621694,0.818212761300913,
310.277225170907));
#16827=CARTESIAN_POINT('Ctrl Pts',(-36.5564689397755,0.906595575798285,
310.27226344708));
#16828=CARTESIAN_POINT('Ctrl Pts',(-36.5267159943775,0.99381916317762,310.267301723252));
#16829=CARTESIAN_POINT('Ctrl Pts',(-36.4929364206862,1.0794620572737,310.262339999425));
#16830=CARTESIAN_POINT('Ctrl Pts',(-36.4591593905128,1.16509850267292,310.257378649203));
#16831=CARTESIAN_POINT('Ctrl Pts',(-36.4213565034685,1.24915406511091,310.252417298981));
#16832=CARTESIAN_POINT('Ctrl Pts',(-36.3797125300232,1.33122616379923,310.247455948759));
#16833=CARTESIAN_POINT('Ctrl Pts',(-36.3368159693807,1.41576686602291,310.242345368691));
#16834=CARTESIAN_POINT('Ctrl Pts',(-36.289843781522,1.49820241227349,310.237234788622));
#16835=CARTESIAN_POINT('Ctrl Pts',(-36.2390485695323,1.57812059265973,310.232124208554));
#16836=CARTESIAN_POINT('Ctrl Pts',(-36.189671218157,1.6558079950668,310.227156281501));
#16837=CARTESIAN_POINT('Ctrl Pts',(-36.1366817872867,1.73111637604713,310.222188354449));
#16838=CARTESIAN_POINT('Ctrl Pts',(-36.0803549698273,1.80369855066789,310.217220427397));
#16839=CARTESIAN_POINT('Ctrl Pts',(-36.0216020326857,1.87940699888914,310.21203852082));
#16840=CARTESIAN_POINT('Ctrl Pts',(-35.9592181044242,1.95214867708126,310.206856614243));
#16841=CARTESIAN_POINT('Ctrl Pts',(-35.8935582465988,2.02157160992029,310.201674707667));
#16842=CARTESIAN_POINT('Ctrl Pts',(-35.8278983887735,2.09099454275932,310.19649280109));
#16843=CARTESIAN_POINT('Ctrl Pts',(-35.7589630590051,2.15709840293153,310.191310894513));
#16844=CARTESIAN_POINT('Ctrl Pts',(-35.6871451388127,2.21957947483799,310.186128987937));
#16845=CARTESIAN_POINT('Ctrl Pts',(-35.6171238025698,2.28049753168308,310.181076710987));
#16846=CARTESIAN_POINT('Ctrl Pts',(-35.5440912695704,2.33820822865127,310.176024434037));
#16847=CARTESIAN_POINT('Ctrl Pts',(-35.4683736292143,2.39239954172348,310.170972157087));
#16848=CARTESIAN_POINT('Ctrl Pts',(-35.3927604175115,2.44651611493563,310.165926848163));
#16849=CARTESIAN_POINT('Ctrl Pts',(-35.3144698154288,2.49712269321811,310.160881539239));
#16850=CARTESIAN_POINT('Ctrl Pts',(-35.2338623888242,2.54394618560706,310.155836230315));
#16851=CARTESIAN_POINT('Ctrl Pts',(-35.1533412283792,2.59071956744122,310.150796320886));
#16852=CARTESIAN_POINT('Ctrl Pts',(-35.0705085538136,2.63371768876335,310.145756411457));
#16853=CARTESIAN_POINT('Ctrl Pts',(-34.9857545271178,2.67271027361161,310.140716502029));
#16854=CARTESIAN_POINT('Ctrl Pts',(-34.9010615939771,2.71167475129226,310.135680225536));
#16855=CARTESIAN_POINT('Ctrl Pts',(-34.8144504639697,2.7466392463159,310.130643949044));
#16856=CARTESIAN_POINT('Ctrl Pts',(-34.7263356284558,2.77741953371835,310.125607672552));
#16857=CARTESIAN_POINT('Ctrl Pts',(-34.6382528337535,2.80818862861973,310.120573227378));
#16858=CARTESIAN_POINT('Ctrl Pts',(-34.548667838774,2.83477639213302,310.115538782205));
#16859=CARTESIAN_POINT('Ctrl Pts',(-34.4580138578032,2.85704722997347,310.110504337032));
#16860=CARTESIAN_POINT('Ctrl Pts',(-34.3673674808716,2.87931619974016,310.105470314147));
#16861=CARTESIAN_POINT('Ctrl Pts',(-34.2756527276982,2.89726885796853,310.100436291262));
#16862=CARTESIAN_POINT('Ctrl Pts',(-34.1833155560286,2.91082015232438,310.095402268377));
#16863=CARTESIAN_POINT('Ctrl Pts',(-34.0909602989637,2.92437410087151,310.090367259516));
#16864=CARTESIAN_POINT('Ctrl Pts',(-33.9979828208674,2.93352490934959,310.085332250654));
#16865=CARTESIAN_POINT('Ctrl Pts',(-33.9048356530551,2.93823922511741,310.080297241793));
#16866=CARTESIAN_POINT('Ctrl Pts',(-33.8115861350909,2.94295872097762,310.075256700461));
#16867=CARTESIAN_POINT('Ctrl Pts',(-33.7181669995994,2.94323197091792,310.070216159129));
#16868=CARTESIAN_POINT('Ctrl Pts',(-33.6250319325769,2.93907775954891,310.065175617798));
#16869=CARTESIAN_POINT('Ctrl Pts',(-33.531839644804,2.93492099589643,310.060131979635));
#16870=CARTESIAN_POINT('Ctrl Pts',(-33.4389322149921,2.92633139648946,310.055088341473));
#16871=CARTESIAN_POINT('Ctrl Pts',(-33.3467571692897,2.9133795360414,310.05004470331));
#16872=CARTESIAN_POINT('Ctrl Pts',(-33.2544328719875,2.9004067036928,310.044992898392));
#16873=CARTESIAN_POINT('Ctrl Pts',(-33.1628437622273,2.88305759155797,310.039941093474));
#16874=CARTESIAN_POINT('Ctrl Pts',(-33.0724259801845,2.86145363075587,310.034889288556));
#16875=CARTESIAN_POINT('Ctrl Pts',(-33.0266569652171,2.85051781721382,310.03233209096));
#16876=CARTESIAN_POINT('Ctrl Pts',(-32.9811878275027,2.83849256113045,310.029774893363));
#16877=CARTESIAN_POINT('Ctrl Pts',(-32.9360732888412,2.82539835587649,310.027217695767));
#16878=CARTESIAN_POINT('Ctrl Pts',(-32.846940112708,2.79952802365425,310.022165418817));
#16879=CARTESIAN_POINT('Ctrl Pts',(-32.7588723470157,2.76938927675331,310.017113141868));
#16880=CARTESIAN_POINT('Ctrl Pts',(-32.6723088992443,2.73508725084322,310.012060864919));
#16881=CARTESIAN_POINT('Ctrl Pts',(-32.585864838504,2.70083253378158,310.007015555995));
#16882=CARTESIAN_POINT('Ctrl Pts',(-32.5009213823539,2.6624261099013,310.001970247071));
#16883=CARTESIAN_POINT('Ctrl Pts',(-32.4179033815805,2.62002318300882,309.996924938148));
#16884=CARTESIAN_POINT('Ctrl Pts',(-32.3349742267663,2.57766563577707,309.99188502872));
#16885=CARTESIAN_POINT('Ctrl Pts',(-32.2539668250374,2.53132028783144,309.986845119292));
#16886=CARTESIAN_POINT('Ctrl Pts',(-32.1752860640212,2.48119041092724,309.981805209864));
#16887=CARTESIAN_POINT('Ctrl Pts',(-32.0966620187463,2.43109666932591,309.976768933372));
#16888=CARTESIAN_POINT('Ctrl Pts',(-32.0203616542664,2.37722405910684,309.97173265688));
#16889=CARTESIAN_POINT('Ctrl Pts',(-31.9467643223076,2.31982124509054,309.966696380388));
#16890=CARTESIAN_POINT('Ctrl Pts',(-31.8731937522243,2.26243930420819,309.961661935216));
#16891=CARTESIAN_POINT('Ctrl Pts',(-31.8023246119943,2.20152998262774,309.956627490043));
#16892=CARTESIAN_POINT('Ctrl Pts',(-31.7345055124579,2.13738402234726,309.95159304487));
#16893=CARTESIAN_POINT('Ctrl Pts',(-31.6666921015751,2.07324344261824,309.946559021986));
#16894=CARTESIAN_POINT('Ctrl Pts',(-31.6019285453523,2.00586706937989,309.941524999102));
#16895=CARTESIAN_POINT('Ctrl Pts',(-31.5405278686293,1.93558373033768,309.936490976218));
#16896=CARTESIAN_POINT('Ctrl Pts',(-31.4791151658125,1.86528662542069,309.931455967357));
#16897=CARTESIAN_POINT('Ctrl Pts',(-31.4210669425874,1.79208175872728,309.926420958496));
#16898=CARTESIAN_POINT('Ctrl Pts',(-31.3666563229955,1.71633148401794,309.921385949635));
#16899=CARTESIAN_POINT('Ctrl Pts',(-31.3121859169892,1.64049797487098,309.916345408304));
#16900=CARTESIAN_POINT('Ctrl Pts',(-31.2613613526787,1.56211383615331,309.911304866973));
#16901=CARTESIAN_POINT('Ctrl Pts',(-31.2144125506615,1.48157062930825,309.906264325642));
#16902=CARTESIAN_POINT('Ctrl Pts',(-31.1674349040235,1.40097793795746,309.90122068748));
#16903=CARTESIAN_POINT('Ctrl Pts',(-31.1243379652487,1.31822393141491,309.896177049318));
#16904=CARTESIAN_POINT('Ctrl Pts',(-31.0853047818433,1.23372304188724,309.891133411156));
#16905=CARTESIAN_POINT('Ctrl Pts',(-31.0462083951598,1.14908532690086,309.886081606239));
#16906=CARTESIAN_POINT('Ctrl Pts',(-31.0111890669144,1.06269549320429,309.881029801322));
#16907=CARTESIAN_POINT('Ctrl Pts',(-30.980380926012,0.974985944782278,309.875977996404));
#16908=CARTESIAN_POINT('Ctrl Pts',(-30.9647860039348,0.930587823603603,
309.873420798802));
#16909=CARTESIAN_POINT('Ctrl Pts',(-30.9502693244297,0.885851761032472,
309.8708636012));
#16910=CARTESIAN_POINT('Ctrl Pts',(-30.9368432966644,0.840834857561148,
309.868306403598));
#16911=CARTESIAN_POINT('Ctrl Pts',(-30.9103173799509,0.751894580283191,
309.863254126648));
#16912=CARTESIAN_POINT('Ctrl Pts',(-30.8879566910281,0.661538202464539,
309.858201849698));
#16913=CARTESIAN_POINT('Ctrl Pts',(-30.8699105561981,0.570191628954484,
309.853149572748));
#16914=CARTESIAN_POINT('Ctrl Pts',(-30.8518893103312,0.478971039291871,
309.848104263823));
#16915=CARTESIAN_POINT('Ctrl Pts',(-30.8381708793757,0.386763399734169,
309.843058954899));
#16916=CARTESIAN_POINT('Ctrl Pts',(-30.8288548872494,0.294009914868297,
309.838013645975));
#16917=CARTESIAN_POINT('Ctrl Pts',(-30.8195488651085,0.201355694887732,
309.832973736546));
#16918=CARTESIAN_POINT('Ctrl Pts',(-30.8146359611485,0.108157230370923,
309.827933827117));
#16919=CARTESIAN_POINT('Ctrl Pts',(-30.8141645794648,0.0148649771324433,
309.822893917688));
#16920=CARTESIAN_POINT('Ctrl Pts',(-30.813693537569,-0.0783600279098104,
309.817857641196));
#16921=CARTESIAN_POINT('Ctrl Pts',(-30.8176576565629,-0.171678244323985,
309.812821364703));
#16922=CARTESIAN_POINT('Ctrl Pts',(-30.8260533512008,-0.264636098443424,
309.80778508821));
#16923=CARTESIAN_POINT('Ctrl Pts',(-30.834445992949,-0.357560150705554,
309.802750643037));
#16924=CARTESIAN_POINT('Ctrl Pts',(-30.8472669691344,-0.450123658982208,
309.797716197864));
#16925=CARTESIAN_POINT('Ctrl Pts',(-30.8644606736798,-0.541876103138771,
309.79268175269));
#16926=CARTESIAN_POINT('Ctrl Pts',(-30.8816529360205,-0.633620851117278,
309.787647729805));
#16927=CARTESIAN_POINT('Ctrl Pts',(-30.9032171154638,-0.724554233616771,
309.78261370692));
#16928=CARTESIAN_POINT('Ctrl Pts',(-30.9290463164374,-0.814235018785542,
309.777579684035));
#16929=CARTESIAN_POINT('Ctrl Pts',(-30.9548805763844,-0.903933369062518,
309.772544675173));
#16930=CARTESIAN_POINT('Ctrl Pts',(-30.9849813935838,-0.992378207993662,
309.767509666312));
#16931=CARTESIAN_POINT('Ctrl Pts',(-31.0191920791562,-1.07914368867578,
309.76247465745));
#16932=CARTESIAN_POINT('Ctrl Pts',(-31.053440355446,-1.16600450730914,309.757434116118));
#16933=CARTESIAN_POINT('Ctrl Pts',(-31.0918073512228,-1.25118187036631,
309.752393574786));
#16934=CARTESIAN_POINT('Ctrl Pts',(-31.1340884258291,-1.33427043102484,
309.747353033455));
#16935=CARTESIAN_POINT('Ctrl Pts',(-31.1763954772765,-1.41741004001541,
309.742309395292));
#16936=CARTESIAN_POINT('Ctrl Pts',(-31.2226211750026,-1.49845790613682,
309.737265757129));
#16937=CARTESIAN_POINT('Ctrl Pts',(-31.2725162662144,-1.57703569952134,
309.732222118966));
#16938=CARTESIAN_POINT('Ctrl Pts',(-31.3224921485133,-1.6557407275737,309.727170314048));
#16939=CARTESIAN_POINT('Ctrl Pts',(-31.3761490304801,-1.73196733537553,
309.72211850913));
#16940=CARTESIAN_POINT('Ctrl Pts',(-31.4331960576555,-1.80536858279825,
309.717066704211));
#16941=CARTESIAN_POINT('Ctrl Pts',(-31.4620729685833,-1.84252391566604,
309.714509506617));
#16942=CARTESIAN_POINT('Ctrl Pts',(-31.4918179327893,-1.87895585727067,
309.711952309023));
#16943=CARTESIAN_POINT('Ctrl Pts',(-31.5223896698333,-1.91462305088546,
309.709395111429));
#16944=CARTESIAN_POINT('Ctrl Pts',(-31.5827905096962,-1.98509102746098,
309.704342834479));
#16945=CARTESIAN_POINT('Ctrl Pts',(-31.6466376295842,-2.0528244808105,309.699290557529));
#16946=CARTESIAN_POINT('Ctrl Pts',(-31.7136538692465,-2.11746721508837,
309.694238280579));
#16947=CARTESIAN_POINT('Ctrl Pts',(-31.780577681099,-2.18202079506008,309.689192971655));
#16948=CARTESIAN_POINT('Ctrl Pts',(-31.8506616104126,-2.24349182068772,
309.684147662731));
#16949=CARTESIAN_POINT('Ctrl Pts',(-31.9235887170129,-2.30155759189633,
309.679102353807));
#16950=CARTESIAN_POINT('Ctrl Pts',(-31.9964377769405,-2.35956122105036,
309.674062444378));
#16951=CARTESIAN_POINT('Ctrl Pts',(-32.0721236205085,-2.4141665641599,309.669022534949));
#16952=CARTESIAN_POINT('Ctrl Pts',(-32.1502937904264,-2.46508896835621,
309.663982625521));
#16953=CARTESIAN_POINT('Ctrl Pts',(-32.2284076126545,-2.51597466596951,
309.658946349028));
#16954=CARTESIAN_POINT('Ctrl Pts',(-32.3090018306251,-2.56318245963682,
309.653910072536));
#16955=CARTESIAN_POINT('Ctrl Pts',(-32.3916932091461,-2.60646971236028,
309.648873796044));
#16956=CARTESIAN_POINT('Ctrl Pts',(-32.4743545189634,-2.64974122472964,
309.643839350871));
#16957=CARTESIAN_POINT('Ctrl Pts',(-32.5591110811894,-2.68909482245053,
309.638804905698));
#16958=CARTESIAN_POINT('Ctrl Pts',(-32.6455540536062,-2.72433325322679,
309.633770460524));
#16959=CARTESIAN_POINT('Ctrl Pts',(-32.7319897752024,-2.75956872821,309.62873643764));
#16960=CARTESIAN_POINT('Ctrl Pts',(-32.8201112142855,-2.79068955501337,
309.623702414755));
#16961=CARTESIAN_POINT('Ctrl Pts',(-32.9094895588942,-2.81754662792824,
309.61866839187));
#16962=CARTESIAN_POINT('Ctrl Pts',(-32.9988854093746,-2.84440896113825,
309.613633383009));
#16963=CARTESIAN_POINT('Ctrl Pts',(-33.0895382287521,-2.8670057544445,309.608598374147));
#16964=CARTESIAN_POINT('Ctrl Pts',(-33.1810051707611,-2.88523809285828,
309.603563365286));
#16965=CARTESIAN_POINT('Ctrl Pts',(-33.272572616689,-2.9034904649741,309.598522823954));
#16966=CARTESIAN_POINT('Ctrl Pts',(-33.3649555345335,-2.91736872250081,
309.593482282623));
#16967=CARTESIAN_POINT('Ctrl Pts',(-33.4577023410775,-2.92682536340521,
309.588441741291));
#16968=CARTESIAN_POINT('Ctrl Pts',(-33.5505061298309,-2.93628781432411,
309.583398103129));
#16969=CARTESIAN_POINT('Ctrl Pts',(-33.6436738090824,-2.94132321649817,
309.578354464966));
#16970=CARTESIAN_POINT('Ctrl Pts',(-33.7367523457436,-2.94193620287622,
309.573310826804));
#16971=CARTESIAN_POINT('Ctrl Pts',(-33.8299815969541,-2.94255018181355,
309.568259021886));
#16972=CARTESIAN_POINT('Ctrl Pts',(-33.9231209740874,-2.9387274673719,309.563207216968));
#16973=CARTESIAN_POINT('Ctrl Pts',(-34.0157213005729,-2.93052466500855,
309.55815541205));
#16974=CARTESIAN_POINT('Ctrl Pts',(-34.0625951082925,-2.92637244875475,
309.555598214453));
#16975=CARTESIAN_POINT('Ctrl Pts',(-34.1093309311938,-2.9210987283285,309.553041016856));
#16976=CARTESIAN_POINT('Ctrl Pts',(-34.1558716459712,-2.914715807452,309.550483819259));
#16977=CARTESIAN_POINT('Ctrl Pts',(-34.2478225303235,-2.90210501661753,
309.545431542309));
#16978=CARTESIAN_POINT('Ctrl Pts',(-34.33934112768,-2.88511614501201,309.540379265359));
#16979=CARTESIAN_POINT('Ctrl Pts',(-34.4299778973623,-2.86378927335161,
309.535326988409));
#16980=CARTESIAN_POINT('Ctrl Pts',(-34.5204896621479,-2.84249181539825,
309.530281679485));
#16981=CARTESIAN_POINT('Ctrl Pts',(-34.6101215873175,-2.81686834705408,
309.525236370561));
#16982=CARTESIAN_POINT('Ctrl Pts',(-34.6984307457689,-2.78701053071398,
309.520191061637));
#16983=CARTESIAN_POINT('Ctrl Pts',(-34.7866453956583,-2.75718466824293,
309.515151152209));
#16984=CARTESIAN_POINT('Ctrl Pts',(-34.8735396740097,-2.72313360655017,
309.51011124278));
#16985=CARTESIAN_POINT('Ctrl Pts',(-34.9586834021217,-2.68499947122222,
309.505071333352));
#16986=CARTESIAN_POINT('Ctrl Pts',(-35.0437657557684,-2.64689282426267,
309.500035056859));
#16987=CARTESIAN_POINT('Ctrl Pts',(-35.1270996630077,-2.60470913479231,
309.494998780367));
#16988=CARTESIAN_POINT('Ctrl Pts',(-35.2082735964798,-2.55863915699102,
309.489962503875));
#16989=CARTESIAN_POINT('Ctrl Pts',(-35.28941801303,-2.51258593141394,309.484928058702));
#16990=CARTESIAN_POINT('Ctrl Pts',(-35.3684036301592,-2.46264944394667,
309.479893613529));
#16991=CARTESIAN_POINT('Ctrl Pts',(-35.444843204326,-2.4090665550276,309.474859168356));
#16992=CARTESIAN_POINT('Ctrl Pts',(-35.5212763667557,-2.35548816063126,
309.469825145471));
#16993=CARTESIAN_POINT('Ctrl Pts',(-35.5951635471574,-2.29826422805756,
309.464791122586));
#16994=CARTESIAN_POINT('Ctrl Pts',(-35.6661471606637,-2.23767448087141,
309.459757099701));
#16995=CARTESIAN_POINT('Ctrl Pts',(-35.7371446772024,-2.1770728664222,309.45472209084));
#16996=CARTESIAN_POINT('Ctrl Pts',(-35.8052371597658,-2.1131044168001,309.449687081979));
#16997=CARTESIAN_POINT('Ctrl Pts',(-35.870101615119,-2.04608783619383,309.444652073117));
#16998=CARTESIAN_POINT('Ctrl Pts',(-35.9350373435661,-1.97899761773734,
309.439611531786));
#16999=CARTESIAN_POINT('Ctrl Pts',(-35.9967376552072,-1.90885290243591,
309.434570990454));
#17000=CARTESIAN_POINT('Ctrl Pts',(-36.0549180448958,-1.83600758387068,
309.429530449123));
#17001=CARTESIAN_POINT('Ctrl Pts',(-36.1131341797196,-1.76311751026394,
309.42448681096));
#17002=CARTESIAN_POINT('Ctrl Pts',(-36.1678258270901,-1.6875238898987,309.419443172798));
#17003=CARTESIAN_POINT('Ctrl Pts',(-36.2187515235251,-1.60961007095911,
309.414399534635));
#17004=CARTESIAN_POINT('Ctrl Pts',(-36.2697596798232,-1.53157009247136,
309.409347729718));
#17005=CARTESIAN_POINT('Ctrl Pts',(-36.3169894866719,-1.45120279773392,
309.4042959248));
#17006=CARTESIAN_POINT('Ctrl Pts',(-36.3602452595575,-1.36891644076131,
309.399244119882));
#17007=CARTESIAN_POINT('Ctrl Pts',(-36.382141108722,-1.32726351121299,309.396686922284));
#17008=CARTESIAN_POINT('Ctrl Pts',(-36.4030194422427,-1.28511918230115,
309.394129724687));
#17009=CARTESIAN_POINT('Ctrl Pts',(-36.4228596657514,-1.24253813789557,
309.39157252709));
#17010=CARTESIAN_POINT('Ctrl Pts',(-36.4654479700165,-1.15113521220403,
309.386083339466));
#17011=CARTESIAN_POINT('Ctrl Pts',(-36.5033835448867,-1.05743256682659,
309.380594151842));
#17012=CARTESIAN_POINT('Ctrl Pts',(-36.5364336150382,-0.961903980042877,
309.375104964218));
#17013=CARTESIAN_POINT('Ctrl Pts',(-36.5693605733763,-0.866731238118326,
309.369636223868));
#17014=CARTESIAN_POINT('Ctrl Pts',(-36.5974381969507,-0.76974641445008,
309.364167483518));
#17015=CARTESIAN_POINT('Ctrl Pts',(-36.6204819709492,-0.671442287238291,
309.358698743169));
#17016=CARTESIAN_POINT('Ctrl Pts',(-36.6434698437343,-0.573376633116905,
309.353243269275));
#17017=CARTESIAN_POINT('Ctrl Pts',(-36.6614481150749,-0.473998359607168,
309.347787795382));
#17018=CARTESIAN_POINT('Ctrl Pts',(-36.6742814338892,-0.373816595918416,
309.342332321488));
#17019=CARTESIAN_POINT('Ctrl Pts',(-36.6870702578002,-0.273982176353674,
309.336895762483));
#17020=CARTESIAN_POINT('Ctrl Pts',(-36.6947496328921,-0.173350134536088,
309.331459203477));
#17021=CARTESIAN_POINT('Ctrl Pts',(-36.6972350637744,-0.0724396698782973,
309.326022644471));
#17022=CARTESIAN_POINT('Ctrl Pts',(-36.6978212358865,-0.0486406173166869,
309.324740468693));
#17023=CARTESIAN_POINT('Ctrl Pts',(-36.6981187313625,-0.0248261341478378,
309.323458292915));
#17024=CARTESIAN_POINT('Ctrl Pts',(-36.6981268542406,-0.00100312718012004,
309.322176117137));
#17025=CARTESIAN_POINT('',(-36.6981258228997,0.00265982559600335,308.322176117063));
#17026=CARTESIAN_POINT('Ctrl Pts',(-36.6981268542409,-0.00100312630173672,
309.32217611709));
#17027=CARTESIAN_POINT('Ctrl Pts',(-36.6981595100368,0.094770801544592,
309.317021477685));
#17028=CARTESIAN_POINT('Ctrl Pts',(-36.6935110801844,0.190508962578298,
309.311866838281));
#17029=CARTESIAN_POINT('Ctrl Pts',(-36.6842182670738,0.28573708124698,309.306712198876));
#17030=CARTESIAN_POINT('Ctrl Pts',(-36.6749193130744,0.381028128683565,
309.301554153176));
#17031=CARTESIAN_POINT('Ctrl Pts',(-36.6609699063463,0.475808051227989,
309.296396107476));
#17032=CARTESIAN_POINT('Ctrl Pts',(-36.6424583567241,0.569609905983874,
309.291238061776));
#17033=CARTESIAN_POINT('Ctrl Pts',(-36.623914852552,0.663573681060037,309.286071112282));
#17034=CARTESIAN_POINT('Ctrl Pts',(-36.6007935554482,0.756555609160315,
309.280904162788));
#17035=CARTESIAN_POINT('Ctrl Pts',(-36.5732335547574,0.848100702422635,
309.275737213293));
#17036=CARTESIAN_POINT('Ctrl Pts',(-36.54564865705,0.939728495236683,309.270565596106));
#17037=CARTESIAN_POINT('Ctrl Pts',(-36.5136172032491,1.02991647685934,309.265393978919));
#17038=CARTESIAN_POINT('Ctrl Pts',(-36.4773268787502,1.11822866952695,309.260222361731));
#17039=CARTESIAN_POINT('Ctrl Pts',(-36.4409596088543,1.20672810815648,309.255039779303));
#17040=CARTESIAN_POINT('Ctrl Pts',(-36.4003155984257,1.29334343468067,309.249857196875));
#17041=CARTESIAN_POINT('Ctrl Pts',(-36.355629286909,1.37766178420867,309.244674614448));
#17042=CARTESIAN_POINT('Ctrl Pts',(-36.3211012224824,1.44281259451377,309.240670154605));
#17043=CARTESIAN_POINT('Ctrl Pts',(-36.2841607426211,1.50659252353378,309.236665694763));
#17044=CARTESIAN_POINT('Ctrl Pts',(-36.2449332443537,1.5688236369295,309.232661234921));
#17045=CARTESIAN_POINT('Ctrl Pts',(-36.1954413795066,1.64733830111892,309.227608957971));
#17046=CARTESIAN_POINT('Ctrl Pts',(-36.1421416678632,1.72364961194115,309.222556681021));
#17047=CARTESIAN_POINT('Ctrl Pts',(-36.0852564281067,1.79736480014044,309.217504404071));
#17048=CARTESIAN_POINT('Ctrl Pts',(-36.0284496436342,1.87097832143883,309.212459095147));
#17049=CARTESIAN_POINT('Ctrl Pts',(-35.9680674266596,1.94200248643215,309.207413786223));
#17050=CARTESIAN_POINT('Ctrl Pts',(-35.9043763306642,2.0100718698146,309.202368477299));
#17051=CARTESIAN_POINT('Ctrl Pts',(-35.8407533969525,2.07806840526525,309.19732856787));
#17052=CARTESIAN_POINT('Ctrl Pts',(-35.7738289247213,2.14311612182233,309.192288658442));
#17053=CARTESIAN_POINT('Ctrl Pts',(-35.7039101478962,2.20488206196257,309.187248749013));
#17054=CARTESIAN_POINT('Ctrl Pts',(-35.6340417708788,2.26660347913421,309.182212472521));
#17055=CARTESIAN_POINT('Ctrl Pts',(-35.5611837113706,2.32504752860001,309.177176196028));
#17056=CARTESIAN_POINT('Ctrl Pts',(-35.4856797731719,2.3799183372927,309.172139919536));
#17057=CARTESIAN_POINT('Ctrl Pts',(-35.4102032901396,2.43476919355355,309.167105474363));
#17058=CARTESIAN_POINT('Ctrl Pts',(-35.3320831987663,2.4860491293745,309.16207102919));
#17059=CARTESIAN_POINT('Ctrl Pts',(-35.2516952477261,2.53350344225983,309.157036584017));
#17060=CARTESIAN_POINT('Ctrl Pts',(-35.1713140396124,2.58095377468617,309.152002561132));
#17061=CARTESIAN_POINT('Ctrl Pts',(-35.0886657327134,2.62457889650561,309.146968538247));
#17062=CARTESIAN_POINT('Ctrl Pts',(-35.0041528457329,2.66416882937757,309.141934515362));
#17063=CARTESIAN_POINT('Ctrl Pts',(-34.9196234058418,2.70376651643519,309.136899506501));
#17064=CARTESIAN_POINT('Ctrl Pts',(-34.8332290630134,2.73932725681085,309.131864497639));
#17065=CARTESIAN_POINT('Ctrl Pts',(-34.7453935316089,2.7706886832359,309.126829488778));
#17066=CARTESIAN_POINT('Ctrl Pts',(-34.6574614864811,2.80208456961111,309.121788947446));
#17067=CARTESIAN_POINT('Ctrl Pts',(-34.5680855108015,2.82927178191396,309.116748406114));
#17068=CARTESIAN_POINT('Ctrl Pts',(-34.4777054517754,2.85213754478709,309.111707864783));
#17069=CARTESIAN_POINT('Ctrl Pts',(-34.3872698646333,2.87501735603268,309.10666422662));
#17070=CARTESIAN_POINT('Ctrl Pts',(-34.2958294010936,2.89357034392742,309.101620588458));
#17071=CARTESIAN_POINT('Ctrl Pts',(-34.2038329370239,2.90773510082495,309.096576950295));
#17072=CARTESIAN_POINT('Ctrl Pts',(-34.1116875105174,2.92192279356818,309.091525145377));
#17073=CARTESIAN_POINT('Ctrl Pts',(-34.0189847274179,2.93170802346463,309.086473340459));
#17074=CARTESIAN_POINT('Ctrl Pts',(-33.9261772187974,2.93708136279489,309.081421535541));
#17075=CARTESIAN_POINT('Ctrl Pts',(-33.879198536551,2.93980131945303,309.078864337944));
#17076=CARTESIAN_POINT('Ctrl Pts',(-33.8321930031777,2.94139163438225,309.076307140348));
#17077=CARTESIAN_POINT('Ctrl Pts',(-33.7852189249271,2.94185615919161,309.073749942751));
#17078=CARTESIAN_POINT('Ctrl Pts',(-33.6924118406872,2.9427739247917,309.068697665801));
#17079=CARTESIAN_POINT('Ctrl Pts',(-33.5993946983949,2.93929733732224,309.063645388851));
#17080=CARTESIAN_POINT('Ctrl Pts',(-33.5066180822657,2.93140056753885,309.058593111901));
#17081=CARTESIAN_POINT('Ctrl Pts',(-33.4139694222777,2.92351468886392,309.053547802977));
#17082=CARTESIAN_POINT('Ctrl Pts',(-33.3215610680768,2.91122077924754,309.048502494053));
#17083=CARTESIAN_POINT('Ctrl Pts',(-33.2298445745017,2.89454500431871,309.043457185129));
#17084=CARTESIAN_POINT('Ctrl Pts',(-33.138226236023,2.87788707582326,309.0384172757));
#17085=CARTESIAN_POINT('Ctrl Pts',(-33.0472987211957,2.8568566821027,309.033377366272));
#17086=CARTESIAN_POINT('Ctrl Pts',(-32.9575083231665,2.83153177073301,309.028337456843));
#17087=CARTESIAN_POINT('Ctrl Pts',(-32.8677826490785,2.80622511441183,309.023301180351));
#17088=CARTESIAN_POINT('Ctrl Pts',(-32.7791928889215,2.77663021369273,309.018264903859));
#17089=CARTESIAN_POINT('Ctrl Pts',(-32.6921739669336,2.74287584292164,309.013228627366));
#17090=CARTESIAN_POINT('Ctrl Pts',(-32.6051866872551,2.70913374610451,309.008194182193));
#17091=CARTESIAN_POINT('Ctrl Pts',(-32.5197695247725,2.67123534445736,309.00315973702));
#17092=CARTESIAN_POINT('Ctrl Pts',(-32.4363400949979,2.62935856412087,308.998125291847));
#17093=CARTESIAN_POINT('Ctrl Pts',(-32.3529176632685,2.58748529640099,308.993091268962));
#17094=CARTESIAN_POINT('Ctrl Pts',(-32.2714830297116,2.54163451293453,308.988057246077));
#17095=CARTESIAN_POINT('Ctrl Pts',(-32.1924307111754,2.49203086604598,308.983023223193));
#17096=CARTESIAN_POINT('Ctrl Pts',(-32.1133629092499,2.44241750366028,308.977988214331));
#17097=CARTESIAN_POINT('Ctrl Pts',(-32.0366787251165,2.3890500544749,308.97295320547));
#17098=CARTESIAN_POINT('Ctrl Pts',(-31.96274413107,2.33219677446722,308.967918196608));
#17099=CARTESIAN_POINT('Ctrl Pts',(-31.8887282976564,2.27528102404845,308.962877655277));
#17100=CARTESIAN_POINT('Ctrl Pts',(-31.8174684378227,2.21487206843789,308.957837113945));
#17101=CARTESIAN_POINT('Ctrl Pts',(-31.7492975721632,2.1512785840502,308.952796572614));
#17102=CARTESIAN_POINT('Ctrl Pts',(-31.681084823374,2.08764602880528,308.947752934452));
#17103=CARTESIAN_POINT('Ctrl Pts',(-31.6159651567989,2.02082536764919,308.942709296289));
#17104=CARTESIAN_POINT('Ctrl Pts',(-31.5542333009654,1.95116068710975,308.937665658127));
#17105=CARTESIAN_POINT('Ctrl Pts',(-31.4924014877286,1.88138320418524,308.932613853209));
#17106=CARTESIAN_POINT('Ctrl Pts',(-31.4339687147059,1.80875285408697,308.927562048291));
#17107=CARTESIAN_POINT('Ctrl Pts',(-31.379188047652,1.73364503193103,308.922510243373));
#17108=CARTESIAN_POINT('Ctrl Pts',(-31.3514583564981,1.69562583969344,308.919953045776));
#17109=CARTESIAN_POINT('Ctrl Pts',(-31.3246637482859,1.65697227271581,308.917395848179));
#17110=CARTESIAN_POINT('Ctrl Pts',(-31.2988325632628,1.61773543172227,308.914838650582));
#17111=CARTESIAN_POINT('Ctrl Pts',(-31.2477976722396,1.54021487266135,308.909786373632));
#17112=CARTESIAN_POINT('Ctrl Pts',(-31.2003430973805,1.46013779263423,308.904734096682));
#17113=CARTESIAN_POINT('Ctrl Pts',(-31.1567345837079,1.37786898318173,308.899681819732));
#17114=CARTESIAN_POINT('Ctrl Pts',(-31.1131862142546,1.29571363765866,308.894636510808));
#17115=CARTESIAN_POINT('Ctrl Pts',(-31.0734735716699,1.21137295851321,308.889591201884));
#17116=CARTESIAN_POINT('Ctrl Pts',(-31.0378192175375,1.12524071313107,308.88454589296));
#17117=CARTESIAN_POINT('Ctrl Pts',(-31.0022030207353,1.03920064657573,308.879505983532));
#17118=CARTESIAN_POINT('Ctrl Pts',(-30.9706366486545,0.951373233050796,
308.874466074103));
#17119=CARTESIAN_POINT('Ctrl Pts',(-30.9432962830758,0.862175861316719,
308.869426164674));
#17120=CARTESIAN_POINT('Ctrl Pts',(-30.9159756253531,0.773042786050787,
308.864389888182));
#17121=CARTESIAN_POINT('Ctrl Pts',(-30.8928750491081,0.682542138923517,
308.85935361169));
#17122=CARTESIAN_POINT('Ctrl Pts',(-30.8741218516755,0.591109278768155,
308.854317335197));
#17123=CARTESIAN_POINT('Ctrl Pts',(-30.8553754733859,0.499709665943331,
308.849282890024));
#17124=CARTESIAN_POINT('Ctrl Pts',(-30.8409734226155,0.407378948261623,
308.844248444851));
#17125=CARTESIAN_POINT('Ctrl Pts',(-30.8309923033632,0.314564554214339,
308.839213999678));
#17126=CARTESIAN_POINT('Ctrl Pts',(-30.8210120213254,0.221757945421204,
308.834179976793));
#17127=CARTESIAN_POINT('Ctrl Pts',(-30.815451980834,0.128468182655901,308.829145953908));
#17128=CARTESIAN_POINT('Ctrl Pts',(-30.8143369958528,0.035148583111494,
308.824111931023));
#17129=CARTESIAN_POINT('Ctrl Pts',(-30.8132217924879,-0.0581892942482417,
308.819076922162));
#17130=CARTESIAN_POINT('Ctrl Pts',(-30.8165533786246,-0.151556575790484,
308.814041913301));
#17131=CARTESIAN_POINT('Ctrl Pts',(-30.8243044536866,-0.244500324799556,
308.809006904439));
#17132=CARTESIAN_POINT('Ctrl Pts',(-30.8320640456337,-0.337546200444327,
308.803966363108));
#17133=CARTESIAN_POINT('Ctrl Pts',(-30.8442527829522,-0.430167171201971,
308.798925821776));
#17134=CARTESIAN_POINT('Ctrl Pts',(-30.8607915396068,-0.521916109668268,
308.793885280444));
#17135=CARTESIAN_POINT('Ctrl Pts',(-30.8773404574187,-0.613721417268895,
308.788841642282));
#17136=CARTESIAN_POINT('Ctrl Pts',(-30.8982446156997,-0.70465319333625,
308.783798004119));
#17137=CARTESIAN_POINT('Ctrl Pts',(-30.9233743825601,-0.794277322658978,
308.778754365957));
#17138=CARTESIAN_POINT('Ctrl Pts',(-30.9485448400204,-0.884046573088771,
308.773702561039));
#17139=CARTESIAN_POINT('Ctrl Pts',(-30.9779544256604,-0.972503528671947,
308.768650756121));
#17140=CARTESIAN_POINT('Ctrl Pts',(-31.0114246241131,-1.05923214129474,
308.763598951203));
#17141=CARTESIAN_POINT('Ctrl Pts',(-31.0283670659601,-1.1031337177347,308.761041753606));
#17142=CARTESIAN_POINT('Ctrl Pts',(-31.0463492218567,-1.14659279432876,
308.758484556009));
#17143=CARTESIAN_POINT('Ctrl Pts',(-31.0653434831359,-1.18955787141558,
308.755927358413));
#17144=CARTESIAN_POINT('Ctrl Pts',(-31.1028706060156,-1.27444433810585,
308.750875081463));
#17145=CARTESIAN_POINT('Ctrl Pts',(-31.1444859129757,-1.35770562351071,
308.745822804513));
#17146=CARTESIAN_POINT('Ctrl Pts',(-31.190026669432,-1.43892076356962,308.740770527563));
#17147=CARTESIAN_POINT('Ctrl Pts',(-31.2355046167484,-1.52002389290471,
308.735725218639));
#17148=CARTESIAN_POINT('Ctrl Pts',(-31.2848970400129,-1.59908610046196,
308.730679909715));
#17149=CARTESIAN_POINT('Ctrl Pts',(-31.3379934585911,-1.67570703100534,
308.725634600791));
#17150=CARTESIAN_POINT('Ctrl Pts',(-31.3910330533219,-1.75224596174191,
308.720594691362));
#17151=CARTESIAN_POINT('Ctrl Pts',(-31.4477685125986,-1.82634844532714,
308.715554781933));
#17152=CARTESIAN_POINT('Ctrl Pts',(-31.507944379815,-1.89764032227676,308.710514872505));
#17153=CARTESIAN_POINT('Ctrl Pts',(-31.5680768702405,-1.9688808096414,308.705478596012));
#17154=CARTESIAN_POINT('Ctrl Pts',(-31.6316445536061,-2.03731437877803,
308.70044231952));
#17155=CARTESIAN_POINT('Ctrl Pts',(-31.698350391571,-2.10259823215311,308.695406043028));
#17156=CARTESIAN_POINT('Ctrl Pts',(-31.7650319735841,-2.16785834664651,
308.690371597855));
#17157=CARTESIAN_POINT('Ctrl Pts',(-31.8348491260709,-2.2299707102517,308.685337152681));
#17158=CARTESIAN_POINT('Ctrl Pts',(-31.9074672094207,-2.28862860362045,
308.680302707508));
#17159=CARTESIAN_POINT('Ctrl Pts',(-31.9800792015791,-2.34728157677604,
308.675268684623));
#17160=CARTESIAN_POINT('Ctrl Pts',(-32.0554913117727,-2.40248037679197,
308.670234661739));
#17161=CARTESIAN_POINT('Ctrl Pts',(-32.133335901137,-2.45395863198124,308.665200638854));
#17162=CARTESIAN_POINT('Ctrl Pts',(-32.2111957373415,-2.50544696983323,
308.660165629992));
#17163=CARTESIAN_POINT('Ctrl Pts',(-32.2914886281697,-2.5532130709011,308.655130621131));
#17164=CARTESIAN_POINT('Ctrl Pts',(-32.3738190298947,-2.59703457927613,
308.65009561227));
#17165=CARTESIAN_POINT('Ctrl Pts',(-32.4562398963043,-2.64090423874534,
308.645055070938));
#17166=CARTESIAN_POINT('Ctrl Pts',(-32.5407023497848,-2.6808204446462,308.640014529606));
#17167=CARTESIAN_POINT('Ctrl Pts',(-32.6267876620212,-2.7166075540359,308.634973988275));
#17168=CARTESIAN_POINT('Ctrl Pts',(-32.7129258637477,-2.7524166504744,308.629930350112));
#17169=CARTESIAN_POINT('Ctrl Pts',(-32.800688491616,-2.78409144931917,308.62488671195));
#17170=CARTESIAN_POINT('Ctrl Pts',(-32.8896404024585,-2.81150581228461,
308.619843073787));
#17171=CARTESIAN_POINT('Ctrl Pts',(-32.9787363459386,-2.83896456511163,
308.614791268869));
#17172=CARTESIAN_POINT('Ctrl Pts',(-33.0690249870781,-2.86214899953888,
308.609739463951));
#17173=CARTESIAN_POINT('Ctrl Pts',(-33.1600598958886,-2.8809838557836,308.604687659033));
#17174=CARTESIAN_POINT('Ctrl Pts',(-33.2061412972523,-2.89051796288145,
308.602130461437));
#17175=CARTESIAN_POINT('Ctrl Pts',(-33.2524138128963,-2.89893838835933,
308.59957326384));
#17176=CARTESIAN_POINT('Ctrl Pts',(-33.2988191974236,-2.9062404495502,308.597016066243));
#17177=CARTESIAN_POINT('Ctrl Pts',(-33.3905027086586,-2.92066719368886,
308.591963789293));
#17178=CARTESIAN_POINT('Ctrl Pts',(-33.4830341420085,-2.93077705337546,
308.586911512343));
#17179=CARTESIAN_POINT('Ctrl Pts',(-33.5759714816422,-2.93647884039791,
308.581859235393));
#17180=CARTESIAN_POINT('Ctrl Pts',(-33.668780643467,-2.94217276359974,308.576813926469));
#17181=CARTESIAN_POINT('Ctrl Pts',(-33.7619941595681,-2.9434706680037,308.571768617545));
#17182=CARTESIAN_POINT('Ctrl Pts',(-33.8551614799973,-2.94033266430423,
308.566723308621));
#17183=CARTESIAN_POINT('Ctrl Pts',(-33.9482290926541,-2.93719801889989,
308.561683399192));
#17184=CARTESIAN_POINT('Ctrl Pts',(-34.0412501662869,-2.9296369162686,308.556643489764));
#17185=CARTESIAN_POINT('Ctrl Pts',(-34.1337718136874,-2.91766146318791,
308.551603580335));
#17186=CARTESIAN_POINT('Ctrl Pts',(-34.2262267683699,-2.90569464241692,
308.546567303843));
#17187=CARTESIAN_POINT('Ctrl Pts',(-34.3181825730628,-2.88931985275281,
308.541531027351));
#17188=CARTESIAN_POINT('Ctrl Pts',(-34.4091901845105,-2.86860114167632,
308.536494750858));
#17189=CARTESIAN_POINT('Ctrl Pts',(-34.5001647032592,-2.84788996445394,
308.531460305685));
#17190=CARTESIAN_POINT('Ctrl Pts',(-34.5901912809832,-2.82283810230144,
308.526425860512));
#17191=CARTESIAN_POINT('Ctrl Pts',(-34.6788308388284,-2.79356075151802,
308.521391415339));
#17192=CARTESIAN_POINT('Ctrl Pts',(-34.7674629616039,-2.76428585651336,
308.516357392454));
#17193=CARTESIAN_POINT('Ctrl Pts',(-34.8547078740335,-2.7307863170804,308.511323369569));
#17194=CARTESIAN_POINT('Ctrl Pts',(-34.9401425431737,-2.69322692199041,
308.506289346685));
#17195=CARTESIAN_POINT('Ctrl Pts',(-35.0255939457665,-2.6556601704213,308.501254337823));
#17196=CARTESIAN_POINT('Ctrl Pts',(-35.1092339943976,-2.61403216309768,
308.496219328962));
#17197=CARTESIAN_POINT('Ctrl Pts',(-35.1906615446817,-2.56855498531383,
308.4911843201));
#17198=CARTESIAN_POINT('Ctrl Pts',(-35.2721785675969,-2.52302783718539,
308.486143778769));
#17199=CARTESIAN_POINT('Ctrl Pts',(-35.351477850948,-2.4736432930296,308.481103237437));
#17200=CARTESIAN_POINT('Ctrl Pts',(-35.4281849627321,-2.42065822736884,
308.476062696106));
#17201=CARTESIAN_POINT('Ctrl Pts',(-35.5049392021843,-2.36764060849984,
308.471019057943));
#17202=CARTESIAN_POINT('Ctrl Pts',(-35.5790977466969,-2.3110183336604,308.465975419781));
#17203=CARTESIAN_POINT('Ctrl Pts',(-35.6503188898848,-2.25108888762307,
308.460931781618));
#17204=CARTESIAN_POINT('Ctrl Pts',(-35.7216553557119,-2.19106240267892,
308.4558799767));
#17205=CARTESIAN_POINT('Ctrl Pts',(-35.7900445993316,-2.12771835737363,
308.450828171782));
#17206=CARTESIAN_POINT('Ctrl Pts',(-35.8551815721807,-2.061391279947,308.445776366864));
#17207=CARTESIAN_POINT('Ctrl Pts',(-35.8881535719188,-2.02781685540921,
308.443219169268));
#17208=CARTESIAN_POINT('Ctrl Pts',(-35.9202928687287,-1.99347861331989,
308.440661971671));
#17209=CARTESIAN_POINT('Ctrl Pts',(-35.9515639810421,-1.95842298117019,
308.438104774074));
#17210=CARTESIAN_POINT('Ctrl Pts',(-36.0127391832395,-1.88984418028136,
308.433102167244));
#17211=CARTESIAN_POINT('Ctrl Pts',(-36.0708188799458,-1.81826049345026,
308.428099560414));
#17212=CARTESIAN_POINT('Ctrl Pts',(-36.1254893538265,-1.74398570979198,
308.423096953584));
#17213=CARTESIAN_POINT('Ctrl Pts',(-36.1800900864435,-1.66980567594839,
308.418100728409));
#17214=CARTESIAN_POINT('Ctrl Pts',(-36.231289962854,-1.59294172082055,308.413104503234));
#17215=CARTESIAN_POINT('Ctrl Pts',(-36.2788132813222,-1.51374306058289,
308.408108278059));
#17216=CARTESIAN_POINT('Ctrl Pts',(-36.3262899036055,-1.43462222056899,
308.403116962152));
#17217=CARTESIAN_POINT('Ctrl Pts',(-36.3700969090617,-1.35317161692577,
308.398125646244));
#17218=CARTESIAN_POINT('Ctrl Pts',(-36.4100007259876,-1.26977099532699,
308.393134330336));
#17219=CARTESIAN_POINT('Ctrl Pts',(-36.4498770232938,-1.18642789086733,
308.388146456683));
#17220=CARTESIAN_POINT('Ctrl Pts',(-36.485855284119,-1.10113784771177,308.38315858303));
#17221=CARTESIAN_POINT('Ctrl Pts',(-36.517747532237,-1.01430576032625,308.378170709378));
#17222=CARTESIAN_POINT('Ctrl Pts',(-36.5496347291478,-0.927487425714,308.373183625722));
#17223=CARTESIAN_POINT('Ctrl Pts',(-36.5774370308001,-0.839127953048225,
308.368196542066));
#17224=CARTESIAN_POINT('Ctrl Pts',(-36.6010147219531,-0.749651914684957,
308.36320945841));
#17225=CARTESIAN_POINT('Ctrl Pts',(-36.6245894474414,-0.66018713085516,
308.358223002043));
#17226=CARTESIAN_POINT('Ctrl Pts',(-36.6439405088105,-0.569606500767948,
308.353236545676));
#17227=CARTESIAN_POINT('Ctrl Pts',(-36.6589786081074,-0.478347873358279,
308.348250089309));
#17228=CARTESIAN_POINT('Ctrl Pts',(-36.6740264570508,-0.38703008026958,
308.343260400074));
#17229=CARTESIAN_POINT('Ctrl Pts',(-36.6847556896895,-0.295033860820404,
308.33827071084));
#17230=CARTESIAN_POINT('Ctrl Pts',(-36.691128602081,-0.202804694334924,
308.333281021605));
#17231=CARTESIAN_POINT('Ctrl Pts',(-36.6958563904099,-0.134383860953072,
308.329579386766));
#17232=CARTESIAN_POINT('Ctrl Pts',(-36.6981877482332,-0.0658350003864118,
308.325877751928));
#17233=CARTESIAN_POINT('Ctrl Pts',(-36.6981258229002,0.00265982508757234,
308.32217611709));
#17234=CARTESIAN_POINT('',(-36.6981269972619,-0.000405865267969561,307.322176117036));
#17235=CARTESIAN_POINT('Ctrl Pts',(-36.6981258228997,0.00265982559600865,
308.322176117062));
#17236=CARTESIAN_POINT('Ctrl Pts',(-36.6980207165872,0.118916562715971,
308.31589330686));
#17237=CARTESIAN_POINT('Ctrl Pts',(-36.6910209105583,0.234866416982035,
308.309610496657));
#17238=CARTESIAN_POINT('Ctrl Pts',(-36.6772570076419,0.349805125770544,
308.303327686454));
#17239=CARTESIAN_POINT('Ctrl Pts',(-36.6632385686633,0.46686939781797,308.296928688149));
#17240=CARTESIAN_POINT('Ctrl Pts',(-36.6422035725581,0.582884936325711,
308.290529689843));
#17241=CARTESIAN_POINT('Ctrl Pts',(-36.614338362144,0.69713123132884,308.284130691537));
#17242=CARTESIAN_POINT('Ctrl Pts',(-36.6071718037381,0.72651384619626,308.282484954993));
#17243=CARTESIAN_POINT('Ctrl Pts',(-36.5995537056682,0.755779546793188,
308.280839218449));
#17244=CARTESIAN_POINT('Ctrl Pts',(-36.5914877430168,0.784916301390282,
308.279193481904));
#17245=CARTESIAN_POINT('Ctrl Pts',(-36.5667258956109,0.874363761341445,
308.274141204954));
#17246=CARTESIAN_POINT('Ctrl Pts',(-36.5376827365198,0.962798880669296,
308.269088928004));
#17247=CARTESIAN_POINT('Ctrl Pts',(-36.504457944753,1.04978148056907,308.264036651054));
#17248=CARTESIAN_POINT('Ctrl Pts',(-36.4712789761292,1.1366441153493,308.25899134213));
#17249=CARTESIAN_POINT('Ctrl Pts',(-36.4339299922255,1.22205780008999,308.253946033206));
#17250=CARTESIAN_POINT('Ctrl Pts',(-36.3925609108292,1.30559579005525,308.248900724282));
#17251=CARTESIAN_POINT('Ctrl Pts',(-36.3512361026708,1.38904437756851,308.243860814854));
#17252=CARTESIAN_POINT('Ctrl Pts',(-36.3058999446074,1.47062086428289,308.238820905425));
#17253=CARTESIAN_POINT('Ctrl Pts',(-36.256750666492,1.54991787037237,308.233780995996));
#17254=CARTESIAN_POINT('Ctrl Pts',(-36.2076368168306,1.62915771651067,308.228744719504));
#17255=CARTESIAN_POINT('Ctrl Pts',(-36.1547155437659,1.70612097144661,308.223708443012));
#17256=CARTESIAN_POINT('Ctrl Pts',(-36.0982307837188,1.78042522578225,308.21867216652));
#17257=CARTESIAN_POINT('Ctrl Pts',(-36.0417665629776,1.85470246118737,308.213637721347));
#17258=CARTESIAN_POINT('Ctrl Pts',(-35.9817416980309,1.92632226349075,308.208603276174));
#17259=CARTESIAN_POINT('Ctrl Pts',(-35.9184425808494,1.99493243946904,308.203568831));
#17260=CARTESIAN_POINT('Ctrl Pts',(-35.8551487731861,2.0635368604385,308.198534808116));
#17261=CARTESIAN_POINT('Ctrl Pts',(-35.788581560723,2.12913183060999,308.193500785231));
#17262=CARTESIAN_POINT('Ctrl Pts',(-35.719065859965,2.1914002672259,308.188466762346));
#17263=CARTESIAN_POINT('Ctrl Pts',(-35.6495365436839,2.25368089989717,308.183431753485));
#17264=CARTESIAN_POINT('Ctrl Pts',(-35.5770579233332,2.31263340892541,308.178396744624));
#17265=CARTESIAN_POINT('Ctrl Pts',(-35.5019889342145,2.36798019308723,308.173361735762));
#17266=CARTESIAN_POINT('Ctrl Pts',(-35.426837459255,2.42338779232167,308.168321194431));
#17267=CARTESIAN_POINT('Ctrl Pts',(-35.3490902921085,2.47518149408181,308.163280653099));
#17268=CARTESIAN_POINT('Ctrl Pts',(-35.2691361098323,2.52312653467766,308.158240111768));
#17269=CARTESIAN_POINT('Ctrl Pts',(-35.1891328049381,2.57110103196794,308.153196473606));
#17270=CARTESIAN_POINT('Ctrl Pts',(-35.1069201766292,2.61522195080013,308.148152835443));
#17271=CARTESIAN_POINT('Ctrl Pts',(-35.0229103528424,2.65530111304786,308.143109197281));
#17272=CARTESIAN_POINT('Ctrl Pts',(-34.9387644987399,2.69544517224276,308.138057392363));
#17273=CARTESIAN_POINT('Ctrl Pts',(-34.8528160486947,2.73153423780561,308.133005587445));
#17274=CARTESIAN_POINT('Ctrl Pts',(-34.7654957083083,2.76342882334186,308.127953782527));
#17275=CARTESIAN_POINT('Ctrl Pts',(-34.7212946023161,2.77957369805975,308.12539658493));
#17276=CARTESIAN_POINT('Ctrl Pts',(-34.6767421957652,2.79464460846863,308.122839387332));
#17277=CARTESIAN_POINT('Ctrl Pts',(-34.6318954307013,2.80862843751654,308.120282189735));
#17278=CARTESIAN_POINT('Ctrl Pts',(-34.5432912971566,2.83625640699576,308.115229912785));
#17279=CARTESIAN_POINT('Ctrl Pts',(-34.4532194654202,2.85973704898572,308.110177635835));
#17280=CARTESIAN_POINT('Ctrl Pts',(-34.3621039537994,2.87891576154549,308.105125358886));
#17281=CARTESIAN_POINT('Ctrl Pts',(-34.2711141073492,2.8980680231076,308.100080049962));
#17282=CARTESIAN_POINT('Ctrl Pts',(-34.1790838722977,2.91293005446492,308.095034741038));
#17283=CARTESIAN_POINT('Ctrl Pts',(-34.086453182512,2.92339676230127,308.089989432114));
#17284=CARTESIAN_POINT('Ctrl Pts',(-33.993921626196,2.93385226865497,308.084949522685));
#17285=CARTESIAN_POINT('Ctrl Pts',(-33.9007913315002,2.93992175154603,308.079909613256));
#17286=CARTESIAN_POINT('Ctrl Pts',(-33.8075121186447,2.94155121869017,308.074869703828));
#17287=CARTESIAN_POINT('Ctrl Pts',(-33.7143001445856,2.94317951125954,308.069833427335));
#17288=CARTESIAN_POINT('Ctrl Pts',(-33.6209399086419,2.94037414181107,308.064797150843));
#17289=CARTESIAN_POINT('Ctrl Pts',(-33.5278849940366,2.93313306469108,308.059760874351));
#17290=CARTESIAN_POINT('Ctrl Pts',(-33.4348639165824,2.92589462061226,308.054726429178));
#17291=CARTESIAN_POINT('Ctrl Pts',(-33.3421483823794,2.91422370756339,308.049691984005));
#17292=CARTESIAN_POINT('Ctrl Pts',(-33.2501895671361,2.89817033461967,308.044657538831));
#17293=CARTESIAN_POINT('Ctrl Pts',(-33.1582384653811,2.88211830822991,308.039623515947));
#17294=CARTESIAN_POINT('Ctrl Pts',(-33.0670443939925,2.86168462939915,308.034589493062));
#17295=CARTESIAN_POINT('Ctrl Pts',(-32.9770498778146,2.83697070804971,308.029555470177));
#17296=CARTESIAN_POINT('Ctrl Pts',(-32.8870377350805,2.81225194616841,308.024520461316));
#17297=CARTESIAN_POINT('Ctrl Pts',(-32.7982260424375,2.78325139481809,308.019485452454));
#17298=CARTESIAN_POINT('Ctrl Pts',(-32.7110425590968,2.75012044437866,308.014450443593));
#17299=CARTESIAN_POINT('Ctrl Pts',(-32.6237632785033,2.71695308963519,308.009409902261));
#17300=CARTESIAN_POINT('Ctrl Pts',(-32.5381161943465,2.67964643450673,308.00436936093));
#17301=CARTESIAN_POINT('Ctrl Pts',(-32.4545091626057,2.63840007194239,307.999328819598));
#17302=CARTESIAN_POINT('Ctrl Pts',(-32.3708507639925,2.59712836824825,307.994285181436));
#17303=CARTESIAN_POINT('Ctrl Pts',(-32.2892353013393,2.5519123535183,307.989241543273));
#17304=CARTESIAN_POINT('Ctrl Pts',(-32.2100441695635,2.50299656478565,307.984197905111));
#17305=CARTESIAN_POINT('Ctrl Pts',(-32.1307248099903,2.45400157067097,307.979146100193));
#17306=CARTESIAN_POINT('Ctrl Pts',(-32.0538379840869,2.40129509364048,307.974094295275));
#17307=CARTESIAN_POINT('Ctrl Pts',(-31.9797342158895,2.3451636588574,307.969042490357));
#17308=CARTESIAN_POINT('Ctrl Pts',(-31.9422232705864,2.316750216044,307.96648529276));
#17309=CARTESIAN_POINT('Ctrl Pts',(-31.9054248848701,2.28745980672361,307.963928095163));
#17310=CARTESIAN_POINT('Ctrl Pts',(-31.8693809247322,2.25733319475708,307.961370897566));
#17311=CARTESIAN_POINT('Ctrl Pts',(-31.7981685674183,2.19781179234146,307.956318620616));
#17312=CARTESIAN_POINT('Ctrl Pts',(-31.729647740805,2.13481042932596,307.951266343666));
#17313=CARTESIAN_POINT('Ctrl Pts',(-31.6641780539341,2.06860182282104,307.946214066715));
#17314=CARTESIAN_POINT('Ctrl Pts',(-31.5987986618902,2.00248453025022,307.941168757791));
#17315=CARTESIAN_POINT('Ctrl Pts',(-31.5364623572441,1.93316909716568,307.936123448867));
#17316=CARTESIAN_POINT('Ctrl Pts',(-31.4774957496721,1.86096843334964,307.931078139943));
#17317=CARTESIAN_POINT('Ctrl Pts',(-31.4185922482308,1.78884503876624,307.926038230514));
#17318=CARTESIAN_POINT('Ctrl Pts',(-31.3630515553963,1.71384289310981,307.920998321085));
#17319=CARTESIAN_POINT('Ctrl Pts',(-31.3111626774768,1.63631089285653,307.915958411656));
#17320=CARTESIAN_POINT('Ctrl Pts',(-31.2593112028072,1.55883478027881,307.910922135163));
#17321=CARTESIAN_POINT('Ctrl Pts',(-31.2111065572676,1.47883280591249,307.905885858671));
#17322=CARTESIAN_POINT('Ctrl Pts',(-31.1667961166072,1.39668516334488,307.900849582178));
#17323=CARTESIAN_POINT('Ctrl Pts',(-31.1225017883583,1.31456739176476,307.895815137005));
#17324=CARTESIAN_POINT('Ctrl Pts',(-31.082099062583,1.2303058925807,307.890780691831));
#17325=CARTESIAN_POINT('Ctrl Pts',(-31.0457902517092,1.1443070278345,307.885746246658));
#17326=CARTESIAN_POINT('Ctrl Pts',(-31.0094844864118,1.05831537665717,307.880712223773));
#17327=CARTESIAN_POINT('Ctrl Pts',(-30.9772721258904,0.970587059008257,
307.875678200888));
#17328=CARTESIAN_POINT('Ctrl Pts',(-30.9493075875979,0.881549002821452,
307.870644178003));
#17329=CARTESIAN_POINT('Ctrl Pts',(-30.9213375720993,0.792493507413119,
307.865609169141));
#17330=CARTESIAN_POINT('Ctrl Pts',(-30.8976171639206,0.702128187929003,
307.860574160279));
#17331=CARTESIAN_POINT('Ctrl Pts',(-30.8782507678829,0.610894628588975,
307.855539151418));
#17332=CARTESIAN_POINT('Ctrl Pts',(-30.85886309204,0.519560821770802,307.850498610086));
#17333=CARTESIAN_POINT('Ctrl Pts',(-30.8438390705406,0.427357306001022,
307.845458068754));
#17334=CARTESIAN_POINT('Ctrl Pts',(-30.8332318076716,0.334735040013718,
307.840417527422));
#17335=CARTESIAN_POINT('Ctrl Pts',(-30.8226180278637,0.242055868332932,
307.83537388926));
#17336=CARTESIAN_POINT('Ctrl Pts',(-30.8164264383679,0.148957877202129,
307.830330251097));
#17337=CARTESIAN_POINT('Ctrl Pts',(-30.814658030505,0.0558941223142514,
307.825286612934));
#17338=CARTESIAN_POINT('Ctrl Pts',(-30.8128867592023,-0.0373203231879657,
307.820234808016));
#17339=CARTESIAN_POINT('Ctrl Pts',(-30.8155529550959,-0.13049997825746,
307.815183003098));
#17340=CARTESIAN_POINT('Ctrl Pts',(-30.8226055931285,-0.223194998240111,
307.810131198179));
#17341=CARTESIAN_POINT('Ctrl Pts',(-30.8261756021257,-0.270116739267614,
307.807574000585));
#17342=CARTESIAN_POINT('Ctrl Pts',(-30.8308687418061,-0.316914428363191,
307.805016802991));
#17343=CARTESIAN_POINT('Ctrl Pts',(-30.8366734185194,-0.363530793885804,
307.802459605397));
#17344=CARTESIAN_POINT('Ctrl Pts',(-30.8481417674742,-0.455631142144299,
307.797407328447));
#17345=CARTESIAN_POINT('Ctrl Pts',(-30.8639932262164,-0.547353585824728,
307.792355051498));
#17346=CARTESIAN_POINT('Ctrl Pts',(-30.8841932976764,-0.638248121330135,
307.787302774549));
#17347=CARTESIAN_POINT('Ctrl Pts',(-30.9043655094956,-0.729017296432075,
307.782257465625));
#17348=CARTESIAN_POINT('Ctrl Pts',(-30.9288743206129,-0.818960402425294,
307.777212156702));
#17349=CARTESIAN_POINT('Ctrl Pts',(-30.9576335741544,-0.907633408448775,
307.772166847778));
#17350=CARTESIAN_POINT('Ctrl Pts',(-30.98636204951,-0.996211516520251,307.76712693835));
#17351=CARTESIAN_POINT('Ctrl Pts',(-31.019331789487,-1.08352180604538,307.762087028922));
#17352=CARTESIAN_POINT('Ctrl Pts',(-31.0564060196508,-1.16913236713625,
307.757047119494));
#17353=CARTESIAN_POINT('Ctrl Pts',(-31.0934535254617,-1.25468121725305,
307.752010843002));
#17354=CARTESIAN_POINT('Ctrl Pts',(-31.1345994646829,-1.33853236773558,
307.74697456651));
#17355=CARTESIAN_POINT('Ctrl Pts',(-31.1796582064977,-1.420271954929,307.741938290018));
#17356=CARTESIAN_POINT('Ctrl Pts',(-31.2247005637995,-1.50198181951436,
307.736903844846));
#17357=CARTESIAN_POINT('Ctrl Pts',(-31.2736526829091,-1.5815812574963,307.731869399673));
#17358=CARTESIAN_POINT('Ctrl Pts',(-31.3262825288465,-1.65868011480843,
307.7268349545));
#17359=CARTESIAN_POINT('Ctrl Pts',(-31.3789079602023,-1.73577250508275,
307.721800931616));
#17360=CARTESIAN_POINT('Ctrl Pts',(-31.4352102544216,-1.81036436490036,
307.716766908732));
#17361=CARTESIAN_POINT('Ctrl Pts',(-31.4949141485207,-1.88209466448401,
307.711732885847));
#17362=CARTESIAN_POINT('Ctrl Pts',(-31.5546297363773,-1.95383901334778,
307.706697876986));
#17363=CARTESIAN_POINT('Ctrl Pts',(-31.6177479628078,-2.02272034768013,
307.701662868126));
#17364=CARTESIAN_POINT('Ctrl Pts',(-31.6839541577908,-2.08841174276876,
307.696627859265));
#17365=CARTESIAN_POINT('Ctrl Pts',(-31.7502331001723,-2.15417531959355,
307.691587317934));
#17366=CARTESIAN_POINT('Ctrl Pts',(-31.8196064682104,-2.21674164717348,
307.686546776603));
#17367=CARTESIAN_POINT('Ctrl Pts',(-31.8917239274152,-2.2758218490813,307.681506235272));
#17368=CARTESIAN_POINT('Ctrl Pts',(-31.9638856944762,-2.33493834895518,
307.67646259711));
#17369=CARTESIAN_POINT('Ctrl Pts',(-32.0387945526474,-2.39056419454827,
307.671418958948));
#17370=CARTESIAN_POINT('Ctrl Pts',(-32.1160701807903,-2.44245318213392,
307.666375320786));
#17371=CARTESIAN_POINT('Ctrl Pts',(-32.1934709351106,-2.49442618936225,
307.661323515868));
#17372=CARTESIAN_POINT('Ctrl Pts',(-32.2732457304435,-2.54265002938284,
307.65627171095));
#17373=CARTESIAN_POINT('Ctrl Pts',(-32.354988773443,-2.58692396473145,307.651219906033));
#17374=CARTESIAN_POINT('Ctrl Pts',(-32.3963666803406,-2.60933520252767,
307.648662708431));
#17375=CARTESIAN_POINT('Ctrl Pts',(-32.4382485800879,-2.63073510326995,
307.646105510829));
#17376=CARTESIAN_POINT('Ctrl Pts',(-32.4805800486849,-2.65110239533602,
307.643548313227));
#17377=CARTESIAN_POINT('Ctrl Pts',(-32.5642146895439,-2.69134222668769,
307.638496036277));
#17378=CARTESIAN_POINT('Ctrl Pts',(-32.649905495541,-2.72769275884674,307.633443759327));
#17379=CARTESIAN_POINT('Ctrl Pts',(-32.7372554911071,-2.75993927413227,
307.628391482377));
#17380=CARTESIAN_POINT('Ctrl Pts',(-32.8244850148468,-2.79214131549923,
307.623346173453));
#17381=CARTESIAN_POINT('Ctrl Pts',(-32.9133687678067,-2.82025043500779,
307.618300864529));
#17382=CARTESIAN_POINT('Ctrl Pts',(-33.0034868169279,-2.84409857719549,
307.613255555605));
#17383=CARTESIAN_POINT('Ctrl Pts',(-33.0935084216101,-2.86792119707424,
307.608215646176));
#17384=CARTESIAN_POINT('Ctrl Pts',(-33.1847612697107,-2.88749179048228,
307.603175736747));
#17385=CARTESIAN_POINT('Ctrl Pts',(-33.2768082036211,-2.90269141784396,
307.598135827319));
#17386=CARTESIAN_POINT('Ctrl Pts',(-33.368788787003,-2.91788008880259,307.593099550826));
#17387=CARTESIAN_POINT('Ctrl Pts',(-33.4615618814021,-2.92870398407821,
307.588063274334));
#17388=CARTESIAN_POINT('Ctrl Pts',(-33.5546790395243,-2.93509500852085,
307.583026997842));
#17389=CARTESIAN_POINT('Ctrl Pts',(-33.647762337862,-2.94148370902325,307.577992552668));
#17390=CARTESIAN_POINT('Ctrl Pts',(-33.7411890086107,-2.94344271052498,
307.572958107495));
#17391=CARTESIAN_POINT('Ctrl Pts',(-33.834505403747,-2.940955768077,307.567923662322));
#17392=CARTESIAN_POINT('Ctrl Pts',(-33.9278139715212,-2.9384690342333,307.562889639437));
#17393=CARTESIAN_POINT('Ctrl Pts',(-34.02101183798,-2.93153710992028,307.557855616552));
#17394=CARTESIAN_POINT('Ctrl Pts',(-34.1136464263757,-2.92019586292155,
307.552821593667));
#17395=CARTESIAN_POINT('Ctrl Pts',(-34.2062991584189,-2.90885239459717,
307.547786584806));
#17396=CARTESIAN_POINT('Ctrl Pts',(-34.2983879524005,-2.89309794278361,
307.542751575945));
#17397=CARTESIAN_POINT('Ctrl Pts',(-34.3894675592989,-2.87301997346699,
307.537716567083));
#17398=CARTESIAN_POINT('Ctrl Pts',(-34.4806472445123,-2.85291994246822,
307.532676025752));
#17399=CARTESIAN_POINT('Ctrl Pts',(-34.5708150946446,-2.82848700682537,
307.52763548442));
#17400=CARTESIAN_POINT('Ctrl Pts',(-34.6595385301776,-2.79985922017128,
307.522594943089));
#17401=CARTESIAN_POINT('Ctrl Pts',(-34.7483164760227,-2.77121384504605,
307.517551304926));
#17402=CARTESIAN_POINT('Ctrl Pts',(-34.8356478250652,-2.73836864437978,
307.512507666764));
#17403=CARTESIAN_POINT('Ctrl Pts',(-34.9211196298216,-2.70150999097007,
307.507464028601));
#17404=CARTESIAN_POINT('Ctrl Pts',(-35.0067298321613,-2.66459165532285,
307.502412223683));
#17405=CARTESIAN_POINT('Ctrl Pts',(-35.0904740804961,-2.62364708804529,
307.497360418765));
#17406=CARTESIAN_POINT('Ctrl Pts',(-35.1719638527412,-2.57890869903166,
307.492308613847));
#17407=CARTESIAN_POINT('Ctrl Pts',(-35.2132135551927,-2.55626235723776,
307.489751416251));
#17408=CARTESIAN_POINT('Ctrl Pts',(-35.2538860418139,-2.5326446075465,307.487194218654));
#17409=CARTESIAN_POINT('Ctrl Pts',(-35.2939339552803,-2.50808968060835,
307.484637021058));
#17410=CARTESIAN_POINT('Ctrl Pts',(-35.3730569571472,-2.45957630346084,
307.479584744106));
#17411=CARTESIAN_POINT('Ctrl Pts',(-35.4500240456981,-2.40722802069595,
307.474532467154));
#17412=CARTESIAN_POINT('Ctrl Pts',(-35.5244397220976,-2.35126225806358,
307.469480190202));
#17413=CARTESIAN_POINT('Ctrl Pts',(-35.5987527654934,-2.29537368258595,
307.464434881275));
#17414=CARTESIAN_POINT('Ctrl Pts',(-35.6705210372082,-2.23587780607041,
307.459389572349));
#17415=CARTESIAN_POINT('Ctrl Pts',(-35.7393758311229,-2.17303662510182,
307.454344263423));
#17416=CARTESIAN_POINT('Ctrl Pts',(-35.8081569365588,-2.11026269683656,
307.449304353992));
#17417=CARTESIAN_POINT('Ctrl Pts',(-35.8740304353281,-2.04415087807459,
307.444264444561));
#17418=CARTESIAN_POINT('Ctrl Pts',(-35.9366595815888,-1.97500424576248,
307.43922453513));
#17419=CARTESIAN_POINT('Ctrl Pts',(-35.9992435826527,-1.90590745667042,
307.434188258635));
#17420=CARTESIAN_POINT('Ctrl Pts',(-36.0585875822009,-1.83378053050454,
307.429151982141));
#17421=CARTESIAN_POINT('Ctrl Pts',(-36.1143914620148,-1.75896357163144,
307.424115705646));
#17422=CARTESIAN_POINT('Ctrl Pts',(-36.1701750501082,-1.68417381812141,
307.419081260471));
#17423=CARTESIAN_POINT('Ctrl Pts',(-36.2224208104377,-1.60669633088304,
307.414046815295));
#17424=CARTESIAN_POINT('Ctrl Pts',(-36.2708693956229,-1.52690366778303,
307.40901237012));
#17425=CARTESIAN_POINT('Ctrl Pts',(-36.3193139169498,-1.44711769767692,
307.403978347233));
#17426=CARTESIAN_POINT('Ctrl Pts',(-36.3639616659837,-1.36501731765078,
307.398944324346));
#17427=CARTESIAN_POINT('Ctrl Pts',(-36.4045976837326,-1.28100240873976,
307.393910301459));
#17428=CARTESIAN_POINT('Ctrl Pts',(-36.4452416605558,-1.1969710444538,307.388875292595));
#17429=CARTESIAN_POINT('Ctrl Pts',(-36.4818721525028,-1.1110248066317,307.383840283732));
#17430=CARTESIAN_POINT('Ctrl Pts',(-36.5143215448634,-1.02358536137261,
307.378805274868));
#17431=CARTESIAN_POINT('Ctrl Pts',(-36.5468065926316,-0.936049837610105,
307.373764733534));
#17432=CARTESIAN_POINT('Ctrl Pts',(-36.5751012154517,-0.847018248450529,
307.3687241922));
#17433=CARTESIAN_POINT('Ctrl Pts',(-36.5990871864318,-0.756929007223363,
307.363683650867));
#17434=CARTESIAN_POINT('Ctrl Pts',(-36.623087894023,-0.666784416554289,
307.358640012702));
#17435=CARTESIAN_POINT('Ctrl Pts',(-36.6427745861121,-0.575581314116294,
307.353596374537));
#17436=CARTESIAN_POINT('Ctrl Pts',(-36.658080287479,-0.483767778879875,
307.348552736372));
#17437=CARTESIAN_POINT('Ctrl Pts',(-36.6734107721307,-0.391805577409473,
307.343500931452));
#17438=CARTESIAN_POINT('Ctrl Pts',(-36.6843460521414,-0.299231410509212,
307.338449126532));
#17439=CARTESIAN_POINT('Ctrl Pts',(-36.6908710815961,-0.206497757338855,
307.333397321612));
#17440=CARTESIAN_POINT('Ctrl Pts',(-36.6941740178253,-0.159556460774516,
307.330840124038));
#17441=CARTESIAN_POINT('Ctrl Pts',(-36.6963477327181,-0.112574291880736,
307.328282926463));
#17442=CARTESIAN_POINT('Ctrl Pts',(-36.6973953537782,-0.0656096002261236,
307.325725728889));
#17443=CARTESIAN_POINT('Ctrl Pts',(-36.6978800833787,-0.0438792464827141,
307.324542524956));
#17444=CARTESIAN_POINT('Ctrl Pts',(-36.6981239984268,-0.0221435009775741,
307.323359321023));
#17445=CARTESIAN_POINT('Ctrl Pts',(-36.6981269972618,-0.000405866257568911,
307.32217611709));
#17446=CARTESIAN_POINT('',(-36.698126022555,-0.00242897115736518,306.322176117119));
#17447=CARTESIAN_POINT('Ctrl Pts',(-36.6981269972619,-0.00040586526797348,
307.322176117036));
#17448=CARTESIAN_POINT('Ctrl Pts',(-36.698139753591,0.0920610758296735,
307.31714303732));
#17449=CARTESIAN_POINT('Ctrl Pts',(-36.6937888801165,0.18470001600166,307.312109957604));
#17450=CARTESIAN_POINT('Ctrl Pts',(-36.6850517529411,0.27706306062714,307.307076877888));
#17451=CARTESIAN_POINT('Ctrl Pts',(-36.6763266285064,0.369299220333856,
307.30205071243));
#17452=CARTESIAN_POINT('Ctrl Pts',(-36.6632272637743,0.461259795437067,
307.297024546972));
#17453=CARTESIAN_POINT('Ctrl Pts',(-36.6457830375716,0.55249627193066,307.291998381513));
#17454=CARTESIAN_POINT('Ctrl Pts',(-36.6276799638658,0.647178640723046,
307.286782383814));
#17455=CARTESIAN_POINT('Ctrl Pts',(-36.6048972960815,0.741080639958951,
307.281566386114));
#17456=CARTESIAN_POINT('Ctrl Pts',(-36.5775271082731,0.833705926307351,
307.276350388414));
#17457=CARTESIAN_POINT('Ctrl Pts',(-36.5511998042163,0.922801919879714,
307.271333135395));
#17458=CARTESIAN_POINT('Ctrl Pts',(-36.5206283477159,1.01071624850131,307.266315882377));
#17459=CARTESIAN_POINT('Ctrl Pts',(-36.4859465319387,1.09701844147827,307.261298629358));
#17460=CARTESIAN_POINT('Ctrl Pts',(-36.4512761743739,1.18329212185186,307.256283033945));
#17461=CARTESIAN_POINT('Ctrl Pts',(-36.412498321883,1.26795430918394,307.251267438531));
#17462=CARTESIAN_POINT('Ctrl Pts',(-36.3697956659223,1.35059255025555,307.246251843117));
#17463=CARTESIAN_POINT('Ctrl Pts',(-36.3270949344648,1.43322706702593,307.241236473744));
#17464=CARTESIAN_POINT('Ctrl Pts',(-36.2804699574415,1.51383742112168,307.236221104371));
#17465=CARTESIAN_POINT('Ctrl Pts',(-36.2301497892036,1.59203497558224,307.231205734998));
#17466=CARTESIAN_POINT('Ctrl Pts',(-36.1798175316409,1.67025131685651,307.226189160692));
#17467=CARTESIAN_POINT('Ctrl Pts',(-36.1257885629022,1.74605333106891,307.221172586386));
#17468=CARTESIAN_POINT('Ctrl Pts',(-36.0683350620437,1.8190816349526,307.216156012079));
#17469=CARTESIAN_POINT('Ctrl Pts',(-36.010817394194,1.89219150055938,307.211133835008));
#17470=CARTESIAN_POINT('Ctrl Pts',(-35.9498678401348,1.96252112227767,307.206111657937));
#17471=CARTESIAN_POINT('Ctrl Pts',(-35.8857983772258,2.02974479494494,307.201089480865));
#17472=CARTESIAN_POINT('Ctrl Pts',(-35.821686349775,2.09701312765286,307.196063967311));
#17473=CARTESIAN_POINT('Ctrl Pts',(-35.7544506125824,2.16117109661215,307.191038453757));
#17474=CARTESIAN_POINT('Ctrl Pts',(-35.6844378236209,2.22193192175536,307.186012940203));
#17475=CARTESIAN_POINT('Ctrl Pts',(-35.6143164860534,2.28278695115715,307.180979635036));
#17476=CARTESIAN_POINT('Ctrl Pts',(-35.5414098575938,2.34023405256001,307.17594632987));
#17477=CARTESIAN_POINT('Ctrl Pts',(-35.4660949213958,2.39402877889483,307.170913024704));
#17478=CARTESIAN_POINT('Ctrl Pts',(-35.4456520988773,2.40863034530928,307.169546828709));
#17479=CARTESIAN_POINT('Ctrl Pts',(-35.4250319892514,2.42296308250054,307.168180632714));
#17480=CARTESIAN_POINT('Ctrl Pts',(-35.4042424375054,2.43702268924837,307.166814436719));
#17481=CARTESIAN_POINT('Ctrl Pts',(-35.3273613944309,2.48901598112855,307.161762159766));
#17482=CARTESIAN_POINT('Ctrl Pts',(-35.2478795816544,2.5374609691507,307.156709882814));
#17483=CARTESIAN_POINT('Ctrl Pts',(-35.1661584636723,2.58208740027949,307.151657605861));
#17484=CARTESIAN_POINT('Ctrl Pts',(-35.0845500542523,2.62665228329191,307.146612296935));
#17485=CARTESIAN_POINT('Ctrl Pts',(-35.0007088632262,2.66740886353554,307.141566988008));
#17486=CARTESIAN_POINT('Ctrl Pts',(-34.9150258647783,2.70412970838266,307.136521679082));
#17487=CARTESIAN_POINT('Ctrl Pts',(-34.8294345643735,2.74081125453949,307.131481769651));
#17488=CARTESIAN_POINT('Ctrl Pts',(-34.7420057805569,2.77346547600108,307.12644186022));
#17489=CARTESIAN_POINT('Ctrl Pts',(-34.6531546828219,2.80191102313487,307.121401950789));
#17490=CARTESIAN_POINT('Ctrl Pts',(-34.5643676319506,2.83033606576025,307.116365674294));
#17491=CARTESIAN_POINT('Ctrl Pts',(-34.4741607268776,2.85455832900194,307.1113293978));
#17492=CARTESIAN_POINT('Ctrl Pts',(-34.3829677126316,2.8744451208281,307.106293121305));
#17493=CARTESIAN_POINT('Ctrl Pts',(-34.2918078585032,2.894324681307,307.10125867613));
#17494=CARTESIAN_POINT('Ctrl Pts',(-34.1996630411661,2.90987180767166,307.096224230954));
#17495=CARTESIAN_POINT('Ctrl Pts',(-34.10697970368,2.92100434748801,307.091189785779));
#17496=CARTESIAN_POINT('Ctrl Pts',(-34.014304140456,2.93213595350886,307.086155762892));
#17497=CARTESIAN_POINT('Ctrl Pts',(-33.9210905880013,2.93885365641507,307.081121740005));
#17498=CARTESIAN_POINT('Ctrl Pts',(-33.8277920205403,2.94112701671504,307.076087717118));
#17499=CARTESIAN_POINT('Ctrl Pts',(-33.734475179384,2.94340082228116,307.071052708254));
#17500=CARTESIAN_POINT('Ctrl Pts',(-33.641073734259,2.94122854601304,307.066017699391));
#17501=CARTESIAN_POINT('Ctrl Pts',(-33.548040925887,2.93463186366684,307.060982690527));
#17502=CARTESIAN_POINT('Ctrl Pts',(-33.4549058930231,2.92802793288311,307.055942149194));
#17503=CARTESIAN_POINT('Ctrl Pts',(-33.3621407492861,2.91698992328303,307.05090160786));
#17504=CARTESIAN_POINT('Ctrl Pts',(-33.2701935698905,2.90159140420477,307.045861066527));
#17505=CARTESIAN_POINT('Ctrl Pts',(-33.1781898995652,2.88618342451375,307.040817428362));
#17506=CARTESIAN_POINT('Ctrl Pts',(-33.087005627893,2.86640969600229,307.035773790198));
#17507=CARTESIAN_POINT('Ctrl Pts',(-32.9970764458735,2.84239445150329,307.030730152033));
#17508=CARTESIAN_POINT('Ctrl Pts',(-32.9070016488019,2.81834032106093,307.025678347113));
#17509=CARTESIAN_POINT('Ctrl Pts',(-32.8181864212957,2.7900310983714,307.020626542193));
#17510=CARTESIAN_POINT('Ctrl Pts',(-32.7310489954841,2.75764012026148,307.015574737274));
#17511=CARTESIAN_POINT('Ctrl Pts',(-32.6869404803156,2.74124397433476,307.013017539699));
#17512=CARTESIAN_POINT('Ctrl Pts',(-32.6432615239701,2.72380270133817,307.010460342125));
#17513=CARTESIAN_POINT('Ctrl Pts',(-32.600063964871,2.70534326849839,307.00790314455));
#17514=CARTESIAN_POINT('Ctrl Pts',(-32.5147181804377,2.66887281024197,307.002850867581));
#17515=CARTESIAN_POINT('Ctrl Pts',(-32.4309467017257,2.62829430803742,306.997798590612));
#17516=CARTESIAN_POINT('Ctrl Pts',(-32.3491724805325,2.58376525812186,306.992746313643));
#17517=CARTESIAN_POINT('Ctrl Pts',(-32.2675110411381,2.53929762201457,306.9877010047));
#17518=CARTESIAN_POINT('Ctrl Pts',(-32.1878417723216,2.4908904757435,306.982655695757));
#17519=CARTESIAN_POINT('Ctrl Pts',(-32.1105676113593,2.43874931375297,306.977610386814));
#17520=CARTESIAN_POINT('Ctrl Pts',(-32.0333761492907,2.38666395329252,306.972570477366));
#17521=CARTESIAN_POINT('Ctrl Pts',(-31.9585750665206,2.3308527672113,306.967530567918));
#17522=CARTESIAN_POINT('Ctrl Pts',(-31.8865416649192,2.27156654765131,306.962490658471));
#17523=CARTESIAN_POINT('Ctrl Pts',(-31.8145601874179,2.21232306359354,306.957454381959));
#17524=CARTESIAN_POINT('Ctrl Pts',(-31.7453427677007,2.14960980644218,306.952418105448));
#17525=CARTESIAN_POINT('Ctrl Pts',(-31.6792358642956,2.08371953619431,306.947381828936));
#17526=CARTESIAN_POINT('Ctrl Pts',(-31.6131529990541,2.01785322533666,306.942347383744));
#17527=CARTESIAN_POINT('Ctrl Pts',(-31.5501787174819,1.94881250970079,306.937312938552));
#17528=CARTESIAN_POINT('Ctrl Pts',(-31.4906238694807,1.87692819552715,306.932278493359));
#17529=CARTESIAN_POINT('Ctrl Pts',(-31.4310740169294,1.80504991099688,306.927244470455));
#17530=CARTESIAN_POINT('Ctrl Pts',(-31.3749433109655,1.73032884438235,306.922210447551));
#17531=CARTESIAN_POINT('Ctrl Pts',(-31.3225026665881,1.65312929950753,306.917176424647));
#17532=CARTESIAN_POINT('Ctrl Pts',(-31.2700517510524,1.57591463413311,306.912141415767));
#17533=CARTESIAN_POINT('Ctrl Pts',(-31.2212925817866,1.49622089408594,306.907106406886));
#17534=CARTESIAN_POINT('Ctrl Pts',(-31.1764524078117,1.41444083230993,306.902071398006));
#17535=CARTESIAN_POINT('Ctrl Pts',(-31.1315629634342,1.3325709105665,306.897030856655));
#17536=CARTESIAN_POINT('Ctrl Pts',(-31.0906013239388,1.24861048123626,306.891990315305));
#17537=CARTESIAN_POINT('Ctrl Pts',(-31.0537483167916,1.16297605995543,306.886949773954));
#17538=CARTESIAN_POINT('Ctrl Pts',(-31.016872667725,1.07728902620675,306.881906135773));
#17539=CARTESIAN_POINT('Ctrl Pts',(-30.9841108322309,0.989926368676627,
306.876862497592));
#17540=CARTESIAN_POINT('Ctrl Pts',(-30.9555943407051,0.901321631135792,
306.87181885941));
#17541=CARTESIAN_POINT('Ctrl Pts',(-30.927031674732,0.812573423112735,306.866767054474));
#17542=CARTESIAN_POINT('Ctrl Pts',(-30.9027281917879,0.722579548320724,
306.861715249537));
#17543=CARTESIAN_POINT('Ctrl Pts',(-30.8827646878,0.63178546808248,306.856663444601));
#17544=CARTESIAN_POINT('Ctrl Pts',(-30.8726592658241,0.585825976488276,
306.854106247194));
#17545=CARTESIAN_POINT('Ctrl Pts',(-30.8636650670121,0.539661560227087,
306.851549049788));
#17546=CARTESIAN_POINT('Ctrl Pts',(-30.8557874967225,0.493350402064106,
306.848991852381));
#17547=CARTESIAN_POINT('Ctrl Pts',(-30.8402237133945,0.401853048842495,
306.843939575486));
#17548=CARTESIAN_POINT('Ctrl Pts',(-30.8289659557546,0.309454249419359,
306.838887298591));
#17549=CARTESIAN_POINT('Ctrl Pts',(-30.8221108921367,0.216594853554895,
306.833835021696));
#17550=CARTESIAN_POINT('Ctrl Pts',(-30.8152652829216,0.123863528001442,
306.828789712827));
#17551=CARTESIAN_POINT('Ctrl Pts',(-30.8128103340577,0.0306733075301457,
306.823744403958));
#17552=CARTESIAN_POINT('Ctrl Pts',(-30.8147915248671,-0.0625257878188257,
306.818699095089));
#17553=CARTESIAN_POINT('Ctrl Pts',(-30.8167705954038,-0.155625141390326,
306.813659185715));
#17554=CARTESIAN_POINT('Ctrl Pts',(-30.8231763597282,-0.248732909191379,
306.808619276341));
#17555=CARTESIAN_POINT('Ctrl Pts',(-30.8340023341004,-0.341396088626811,
306.803579366967));
#17556=CARTESIAN_POINT('Ctrl Pts',(-30.8448205047467,-0.433992473329439,
306.79854309053));
#17557=CARTESIAN_POINT('Ctrl Pts',(-30.8600525009477,-0.526144466667463,
306.793506814092));
#17558=CARTESIAN_POINT('Ctrl Pts',(-30.8796398545442,-0.617402264914443,
306.788470537654));
#17559=CARTESIAN_POINT('Ctrl Pts',(-30.8992200856781,-0.708626879492081,
306.783436092535));
#17560=CARTESIAN_POINT('Ctrl Pts',(-30.9231524348441,-0.798957511002144,
306.778401647416));
#17561=CARTESIAN_POINT('Ctrl Pts',(-30.9513271653086,-0.887953684394656,
306.773367202297));
#17562=CARTESIAN_POINT('Ctrl Pts',(-30.9794995324835,-0.976942392809793,
306.768333179466));
#17563=CARTESIAN_POINT('Ctrl Pts',(-31.0119134391844,-1.0645964421749,306.763299156635));
#17564=CARTESIAN_POINT('Ctrl Pts',(-31.0484093608343,-1.15049078647766,
306.758265133804));
#17565=CARTESIAN_POINT('Ctrl Pts',(-31.0849124306717,-1.23640195427339,
306.753230124997));
#17566=CARTESIAN_POINT('Ctrl Pts',(-31.1254989292363,-1.32055232380034,
306.748195116189));
#17567=CARTESIAN_POINT('Ctrl Pts',(-31.16996176735,-1.40253814878296,306.743160107381));
#17568=CARTESIAN_POINT('Ctrl Pts',(-31.2144734612595,-1.48461405984412,
306.738119566102));
#17569=CARTESIAN_POINT('Ctrl Pts',(-31.2628697847167,-1.5645202876586,306.733079024823));
#17570=CARTESIAN_POINT('Ctrl Pts',(-31.3148985311617,-1.64187924026533,
306.728038483544));
#17571=CARTESIAN_POINT('Ctrl Pts',(-31.3669592432718,-1.71928572102787,
306.722994845434));
#17572=CARTESIAN_POINT('Ctrl Pts',(-31.4226565562559,-1.79414145480618,
306.717951207324));
#17573=CARTESIAN_POINT('Ctrl Pts',(-31.4816972501806,-1.86610106860357,
306.712907569213));
#17574=CARTESIAN_POINT('Ctrl Pts',(-31.5408335439427,-1.93817720080406,
306.707855764347));
#17575=CARTESIAN_POINT('Ctrl Pts',(-31.6033237289251,-2.00734752186671,
306.70280395948));
#17576=CARTESIAN_POINT('Ctrl Pts',(-31.6688370895148,-2.07330285393789,
306.697752154613));
#17577=CARTESIAN_POINT('Ctrl Pts',(-31.7019996220824,-2.10668911023929,
306.695194956479));
#17578=CARTESIAN_POINT('Ctrl Pts',(-31.7359362507718,-2.13925220939775,
306.692637758345));
#17579=CARTESIAN_POINT('Ctrl Pts',(-31.7706009921044,-2.17095609620994,
306.690080560212));
#17580=CARTESIAN_POINT('Ctrl Pts',(-31.8390884013205,-2.23359372125404,
306.685028283221));
#17581=CARTESIAN_POINT('Ctrl Pts',(-31.9106657048742,-2.29309973061691,
306.679976006231));
#17582=CARTESIAN_POINT('Ctrl Pts',(-31.9850146601458,-2.34915410097937,
306.67492372924));
#17583=CARTESIAN_POINT('Ctrl Pts',(-32.0592610744286,-2.40513116197615,
306.669878420275));
#17584=CARTESIAN_POINT('Ctrl Pts',(-32.1362711927408,-2.45766577846476,
306.664833111311));
#17585=CARTESIAN_POINT('Ctrl Pts',(-32.2156913400819,-2.5064759922723,306.659787802347));
#17586=CARTESIAN_POINT('Ctrl Pts',(-32.2950264918837,-2.55523396932897,
306.654747892878));
#17587=CARTESIAN_POINT('Ctrl Pts',(-32.3767661696773,-2.60027523483947,
306.64970798341));
#17588=CARTESIAN_POINT('Ctrl Pts',(-32.4605260485303,-2.64135989768591,
306.644668073941));
#17589=CARTESIAN_POINT('Ctrl Pts',(-32.544225550429,-2.68241494531745,306.63963179741));
#17590=CARTESIAN_POINT('Ctrl Pts',(-32.6299419612168,-2.7195188640592,306.634595520879));
#17591=CARTESIAN_POINT('Ctrl Pts',(-32.7172654908323,-2.7524771955988,306.629559244348));
#17592=CARTESIAN_POINT('Ctrl Pts',(-32.8045572673655,-2.78542354264103,
306.624524799136));
#17593=CARTESIAN_POINT('Ctrl Pts',(-32.8934545865554,-2.81422714045999,
306.619490353925));
#17594=CARTESIAN_POINT('Ctrl Pts',(-32.9835277338843,-2.83874168162049,
306.614455908713));
#17595=CARTESIAN_POINT('Ctrl Pts',(-33.0735933258834,-2.86325416650282,
306.609421885791));
#17596=CARTESIAN_POINT('Ctrl Pts',(-33.1648341212131,-2.8834781935354,306.604387862868));
#17597=CARTESIAN_POINT('Ctrl Pts',(-33.2568064110736,-2.89931766528798,
306.599353839946));
#17598=CARTESIAN_POINT('Ctrl Pts',(-33.3487967148501,-2.91516023939793,
306.594318831047));
#17599=CARTESIAN_POINT('Ctrl Pts',(-33.4415183598488,-2.92661647767775,
306.589283822149));
#17600=CARTESIAN_POINT('Ctrl Pts',(-33.534519782234,-2.93364180326083,306.58424881325));
#17601=CARTESIAN_POINT('Ctrl Pts',(-33.6276233946031,-2.94067484827325,
306.579208271883));
#17602=CARTESIAN_POINT('Ctrl Pts',(-33.7210069543244,-2.94326722859524,
306.574167730515));
#17603=CARTESIAN_POINT('Ctrl Pts',(-33.8142164488815,-2.94142645987675,
306.569127189148));
#17604=CARTESIAN_POINT('Ctrl Pts',(-33.9074832099043,-2.93958456021854,
306.56408355095));
#17605=CARTESIAN_POINT('Ctrl Pts',(-34.0005752499398,-2.93330411913235,
306.559039912753));
#17606=CARTESIAN_POINT('Ctrl Pts',(-34.0930434286844,-2.92264457933255,
306.553996274555));
#17607=CARTESIAN_POINT('Ctrl Pts',(-34.1856613336496,-2.91196777940469,
306.548944469603));
#17608=CARTESIAN_POINT('Ctrl Pts',(-34.2776529227837,-2.89689779674328,
306.543892664651));
#17609=CARTESIAN_POINT('Ctrl Pts',(-34.3685791756897,-2.87754519746104,
306.538840859699));
#17610=CARTESIAN_POINT('Ctrl Pts',(-34.4146055688879,-2.86774901302032,
306.53628366248));
#17611=CARTESIAN_POINT('Ctrl Pts',(-34.4603592237407,-2.85685627741157,
306.533726465261));
#17612=CARTESIAN_POINT('Ctrl Pts',(-34.5057849265722,-2.84488611916129,
306.531169268042));
#17613=CARTESIAN_POINT('Ctrl Pts',(-34.5955328883636,-2.82123657191558,
306.526116990939));
#17614=CARTESIAN_POINT('Ctrl Pts',(-34.684321735225,-2.79329347552173,306.521064713835));
#17615=CARTESIAN_POINT('Ctrl Pts',(-34.7717100848437,-2.76115103699193,
306.516012436732));
#17616=CARTESIAN_POINT('Ctrl Pts',(-34.8589779097587,-2.72905292883226,
306.510967127654));
#17617=CARTESIAN_POINT('Ctrl Pts',(-34.944848662327,-2.69276713934605,306.505921818576));
#17618=CARTESIAN_POINT('Ctrl Pts',(-35.0288937696123,-2.65243827722054,
306.500876509497));
#17619=CARTESIAN_POINT('Ctrl Pts',(-35.1128489317433,-2.61215257508189,
306.495836599914));
#17620=CARTESIAN_POINT('Ctrl Pts',(-35.1949819336989,-2.56783259183184,
306.49079669033));
#17621=CARTESIAN_POINT('Ctrl Pts',(-35.2748829662207,-2.51967148489425,
306.485756780746));
#17622=CARTESIAN_POINT('Ctrl Pts',(-35.3547264033976,-2.47154509409835,
306.480720504099));
#17623=CARTESIAN_POINT('Ctrl Pts',(-35.4323406896227,-2.41958331169321,
306.475684227451));
#17624=CARTESIAN_POINT('Ctrl Pts',(-35.5073404167459,-2.3640253081285,306.470647950803));
#17625=CARTESIAN_POINT('Ctrl Pts',(-35.5823128720508,-2.30848750687431,
306.465613505474));
#17626=CARTESIAN_POINT('Ctrl Pts',(-35.6546723003415,-2.24935634647697,
306.460579060145));
#17627=CARTESIAN_POINT('Ctrl Pts',(-35.7240629802756,-2.18691382476478,
306.455544614817));
#17628=CARTESIAN_POINT('Ctrl Pts',(-35.7934478397329,-2.1244765407193,306.450510591776));
#17629=CARTESIAN_POINT('Ctrl Pts',(-35.8598641158273,-2.05872874490757,
306.445476568736));
#17630=CARTESIAN_POINT('Ctrl Pts',(-35.9229907167373,-1.98999139258114,
306.440442545695));
#17631=CARTESIAN_POINT('Ctrl Pts',(-35.9861296817824,-1.92124057718371,
306.435407536678));
#17632=CARTESIAN_POINT('Ctrl Pts',(-36.0459773918053,-1.8494993698208,306.430372527661));
#17633=CARTESIAN_POINT('Ctrl Pts',(-36.1022518111705,-1.77512323203914,
306.425337518644));
#17634=CARTESIAN_POINT('Ctrl Pts',(-36.1585880648787,-1.70066536974278,
306.420296977159));
#17635=CARTESIAN_POINT('Ctrl Pts',(-36.2113429220369,-1.62356715256605,
306.415256435673));
#17636=CARTESIAN_POINT('Ctrl Pts',(-36.2602768120308,-1.54421431330102,
306.410215894187));
#17637=CARTESIAN_POINT('Ctrl Pts',(-36.3092407662475,-1.46481272088265,
306.405172255871));
#17638=CARTESIAN_POINT('Ctrl Pts',(-36.3543788650403,-1.38315413722627,
306.400128617554));
#17639=CARTESIAN_POINT('Ctrl Pts',(-36.3954978286515,-1.29964832250575,
306.395084979238));
#17640=CARTESIAN_POINT('Ctrl Pts',(-36.4366833728559,-1.21600729361156,
306.390033174168));
#17641=CARTESIAN_POINT('Ctrl Pts',(-36.4738366128949,-1.13051346928265,
306.384981369099));
#17642=CARTESIAN_POINT('Ctrl Pts',(-36.506812726369,-1.04359579038107,306.379929564029));
#17643=CARTESIAN_POINT('Ctrl Pts',(-36.5235050543643,-0.999598537461807,
306.377372367977));
#17644=CARTESIAN_POINT('Ctrl Pts',(-36.539127863107,-0.955236679408074,
306.374815171925));
#17645=CARTESIAN_POINT('Ctrl Pts',(-36.553667329706,-0.910566990938581,
306.372257975873));
#17646=CARTESIAN_POINT('Ctrl Pts',(-36.5880629328898,-0.804893177633095,
306.366208489802));
#17647=CARTESIAN_POINT('Ctrl Pts',(-36.6164932427341,-0.697188268922234,
306.36015900373));
#17648=CARTESIAN_POINT('Ctrl Pts',(-36.6387539381384,-0.588069792741501,
306.354109517659));
#17649=CARTESIAN_POINT('Ctrl Pts',(-36.6607618428289,-0.480190457431459,
306.348128729078));
#17650=CARTESIAN_POINT('Ctrl Pts',(-36.6767394151754,-0.370929531773017,
306.342147940497));
#17651=CARTESIAN_POINT('Ctrl Pts',(-36.6865353244095,-0.260904580760653,
306.336167151916));
#17652=CARTESIAN_POINT('Ctrl Pts',(-36.6941739440284,-0.175109711770168,
306.33150347365));
#17653=CARTESIAN_POINT('Ctrl Pts',(-36.6980546711137,-0.0888506926227376,
306.326839795385));
#17654=CARTESIAN_POINT('Ctrl Pts',(-36.698126022555,-0.00242897115734986,
306.322176117119));
#17655=CARTESIAN_POINT('',(-36.6981265705527,0.00163569045731701,305.322176117057));
#17656=CARTESIAN_POINT('Ctrl Pts',(-36.6981260225555,-0.00242897062730326,
306.32217611709));
#17657=CARTESIAN_POINT('Ctrl Pts',(-36.698202775672,0.0905353448933393,
306.31715937303));
#17658=CARTESIAN_POINT('Ctrl Pts',(-36.6938688627679,0.183566125357343,
306.31214262897));
#17659=CARTESIAN_POINT('Ctrl Pts',(-36.685132115652,0.276212201836619,306.30712588491));
#17660=CARTESIAN_POINT('Ctrl Pts',(-36.6763977473887,0.368833052525131,
306.302110506815));
#17661=CARTESIAN_POINT('Ctrl Pts',(-36.6632629682403,0.46106896195887,306.297095128721));
#17662=CARTESIAN_POINT('Ctrl Pts',(-36.6457875999744,0.552472409200222,
306.292079750626));
#17663=CARTESIAN_POINT('Ctrl Pts',(-36.6283120156875,0.643876986321143,
306.287064310534));
#17664=CARTESIAN_POINT('Ctrl Pts',(-36.6064958205825,0.734448641302927,
306.282048870442));
#17665=CARTESIAN_POINT('Ctrl Pts',(-36.5804500087084,0.82374977095704,306.27703343035));
#17666=CARTESIAN_POINT('Ctrl Pts',(-36.5543964610427,0.913077423682411,
306.272016500637));
#17667=CARTESIAN_POINT('Ctrl Pts',(-36.5241109274419,1.00113337224781,306.266999570923));
#17668=CARTESIAN_POINT('Ctrl Pts',(-36.4897539824691,1.08749605001895,306.26198264121));
#17669=CARTESIAN_POINT('Ctrl Pts',(-36.4553563024659,1.1739611229914,306.256959763215));
#17670=CARTESIAN_POINT('Ctrl Pts',(-36.4168777457047,1.2587285034919,306.25193688522));
#17671=CARTESIAN_POINT('Ctrl Pts',(-36.3745265169867,1.34139781635152,306.246914007225));
#17672=CARTESIAN_POINT('Ctrl Pts',(-36.3321451161448,1.4241260249936,306.2418875508));
#17673=CARTESIAN_POINT('Ctrl Pts',(-36.2858857760911,1.50475280471883,306.236861094376));
#17674=CARTESIAN_POINT('Ctrl Pts',(-36.2360008746042,1.5829054587457,306.231834637951));
#17675=CARTESIAN_POINT('Ctrl Pts',(-36.1860368178904,1.66118212205947,306.22680020576));
#17676=CARTESIAN_POINT('Ctrl Pts',(-36.1324359812999,1.73697646456414,306.22176577357));
#17677=CARTESIAN_POINT('Ctrl Pts',(-36.0754916759822,1.80994795974064,306.216731341379));
#17678=CARTESIAN_POINT('Ctrl Pts',(-36.062730423554,1.82630091487481,306.215603122154));
#17679=CARTESIAN_POINT('Ctrl Pts',(-36.0498014057685,1.84251224957421,306.214474902929));
#17680=CARTESIAN_POINT('Ctrl Pts',(-36.0367081721129,1.85857839022412,306.213346683704));
#17681=CARTESIAN_POINT('Ctrl Pts',(-35.978075374343,1.93052416011187,306.208294406214));
#17682=CARTESIAN_POINT('Ctrl Pts',(-35.9159294711306,1.99982180602581,306.203242128725));
#17683=CARTESIAN_POINT('Ctrl Pts',(-35.8505386944799,2.06610836110437,306.198189851235));
#17684=CARTESIAN_POINT('Ctrl Pts',(-35.7852381038654,2.13230349470184,306.193144541775));
#17685=CARTESIAN_POINT('Ctrl Pts',(-35.7167018420535,2.19549547619006,306.188099232316));
#17686=CARTESIAN_POINT('Ctrl Pts',(-35.6452387402726,2.25535383658378,306.183053922856));
#17687=CARTESIAN_POINT('Ctrl Pts',(-35.5738521184413,2.3151481364445,306.178014012896));
#17688=CARTESIAN_POINT('Ctrl Pts',(-35.4995452213187,2.37161562271623,306.172974102936));
#17689=CARTESIAN_POINT('Ctrl Pts',(-35.4226633308578,2.42446298014973,306.167934192977));
#17690=CARTESIAN_POINT('Ctrl Pts',(-35.3458368595817,2.47727224333955,306.162897915962));
#17691=CARTESIAN_POINT('Ctrl Pts',(-35.2664394493703,2.52646631353897,306.157861638948));
#17692=CARTESIAN_POINT('Ctrl Pts',(-35.1848481936732,2.57179311433115,306.152825361933));
#17693=CARTESIAN_POINT('Ctrl Pts',(-35.1032866067365,2.61710343308762,306.147790916243));
#17694=CARTESIAN_POINT('Ctrl Pts',(-35.019533147073,2.65854906056046,306.142756470554));
#17695=CARTESIAN_POINT('Ctrl Pts',(-34.9339916339833,2.69592265532811,306.137722024864));
#17696=CARTESIAN_POINT('Ctrl Pts',(-34.8484572962066,2.73329311515894,306.132688001469));
#17697=CARTESIAN_POINT('Ctrl Pts',(-34.7611356103776,2.76659204370274,306.127653978074));
#17698=CARTESIAN_POINT('Ctrl Pts',(-34.6724515546702,2.79565973551802,306.122619954679));
#17699=CARTESIAN_POINT('Ctrl Pts',(-34.5837501292006,2.82473312056524,306.117584945314));
#17700=CARTESIAN_POINT('Ctrl Pts',(-34.493686226165,2.84957348500391,306.112549935949));
#17701=CARTESIAN_POINT('Ctrl Pts',(-34.4027000997504,2.87007095022769,306.107514926585));
#17702=CARTESIAN_POINT('Ctrl Pts',(-34.3116139979904,2.89059093801889,306.102474384763));
#17703=CARTESIAN_POINT('Ctrl Pts',(-34.2196040841762,2.90675840339532,306.097433842942));
#17704=CARTESIAN_POINT('Ctrl Pts',(-34.1271206231304,2.91851464795662,306.092393301121));
#17705=CARTESIAN_POINT('Ctrl Pts',(-34.0345803418033,2.93027811535664,306.087349662475));
#17706=CARTESIAN_POINT('Ctrl Pts',(-33.9415663765902,2.93762493154942,306.08230602383));
#17707=CARTESIAN_POINT('Ctrl Pts',(-33.8485317360434,2.94054848105325,306.077262385184));
#17708=CARTESIAN_POINT('Ctrl Pts',(-33.7553464523236,2.94347676441505,306.072210579799));
#17709=CARTESIAN_POINT('Ctrl Pts',(-33.6621408700775,2.94196748977113,306.067158774413));
#17710=CARTESIAN_POINT('Ctrl Pts',(-33.569365432799,2.93606609387158,306.062106969028));
#17711=CARTESIAN_POINT('Ctrl Pts',(-33.5224030828902,2.93307884393437,306.05954977653));
#17712=CARTESIAN_POINT('Ctrl Pts',(-33.4755508324832,2.92896701434898,306.056992584032));
#17713=CARTESIAN_POINT('Ctrl Pts',(-33.4288660923819,2.92374148683042,306.054435391535));
#17714=CARTESIAN_POINT('Ctrl Pts',(-33.3366304507842,2.91341734488777,306.04938311342));
#17715=CARTESIAN_POINT('Ctrl Pts',(-33.2447182739149,2.89870573750591,306.044330835305));
#17716=CARTESIAN_POINT('Ctrl Pts',(-33.1535799591182,2.87963557296523,306.03927855719));
#17717=CARTESIAN_POINT('Ctrl Pts',(-33.0625673407369,2.86059170967151,306.034233247091));
#17718=CARTESIAN_POINT('Ctrl Pts',(-32.9723268946378,2.83720132452903,306.029187936992));
#17719=CARTESIAN_POINT('Ctrl Pts',(-32.8833036871683,2.80954505578512,306.024142626893));
#17720=CARTESIAN_POINT('Ctrl Pts',(-32.794375752273,2.78191838476061,306.019102716281));
#17721=CARTESIAN_POINT('Ctrl Pts',(-32.706662888694,2.75003503553994,306.01406280567));
#17722=CARTESIAN_POINT('Ctrl Pts',(-32.6205986710841,2.71402641049569,306.009022895058));
#17723=CARTESIAN_POINT('Ctrl Pts',(-32.5345964913271,2.67804374162513,306.003986617376));
#17724=CARTESIAN_POINT('Ctrl Pts',(-32.4502410040868,2.63794187841581,305.998950339694));
#17725=CARTESIAN_POINT('Ctrl Pts',(-32.3679483456585,2.59390129987756,305.993914062012));
#17726=CARTESIAN_POINT('Ctrl Pts',(-32.2856856108797,2.54987673558482,305.988879615645));
#17727=CARTESIAN_POINT('Ctrl Pts',(-32.205484606065,2.50191651061977,305.983845169278));
#17728=CARTESIAN_POINT('Ctrl Pts',(-32.1277383357946,2.45024779890302,305.978810722912));
#17729=CARTESIAN_POINT('Ctrl Pts',(-32.0499985868298,2.39858342112345,305.973776698831));
#17730=CARTESIAN_POINT('Ctrl Pts',(-31.9747135329271,2.34321142110991,305.96874267475));
#17731=CARTESIAN_POINT('Ctrl Pts',(-31.9022475932433,2.28440255899752,305.96370865067));
#17732=CARTESIAN_POINT('Ctrl Pts',(-31.8297674601869,2.22558217842415,305.958673640611));
#17733=CARTESIAN_POINT('Ctrl Pts',(-31.7601078826416,2.16332387908309,305.953638630553));
#17734=CARTESIAN_POINT('Ctrl Pts',(-31.6935996665186,2.09793824848428,305.948603620495));
#17735=CARTESIAN_POINT('Ctrl Pts',(-31.6270183712348,2.03248077222038,305.943563077973));
#17736=CARTESIAN_POINT('Ctrl Pts',(-31.5635956666475,1.96388941735336,305.938522535451));
#17737=CARTESIAN_POINT('Ctrl Pts',(-31.5036247560481,1.89251090543911,305.933481992929));
#17738=CARTESIAN_POINT('Ctrl Pts',(-31.4436170002741,1.82108853970131,305.928438353577));
#17739=CARTESIAN_POINT('Ctrl Pts',(-31.3870655295055,1.7468759609875,305.923394714226));
#17740=CARTESIAN_POINT('Ctrl Pts',(-31.3342212498735,1.67025040492765,305.918351074875));
#17741=CARTESIAN_POINT('Ctrl Pts',(-31.2812914039423,1.59350077554707,305.913299268782));
#17742=CARTESIAN_POINT('Ctrl Pts',(-31.2320809671197,1.5143307455475,305.90824746269));
#17743=CARTESIAN_POINT('Ctrl Pts',(-31.1867956989889,1.43314358521891,305.903195656597));
#17744=CARTESIAN_POINT('Ctrl Pts',(-31.1638726413815,1.39204726339045,305.900638470853));
#17745=CARTESIAN_POINT('Ctrl Pts',(-31.1419545771068,1.35043443778714,305.898081285109));
#17746=CARTESIAN_POINT('Ctrl Pts',(-31.1210634514639,1.30835926337743,305.895524099365));
#17747=CARTESIAN_POINT('Ctrl Pts',(-31.0797885279475,1.22523068354963,305.890471827515));
#17748=CARTESIAN_POINT('Ctrl Pts',(-31.0423770702963,1.13999781791052,305.885419555665));
#17749=CARTESIAN_POINT('Ctrl Pts',(-31.0090487077173,1.05305494505269,305.880367283814));
#17750=CARTESIAN_POINT('Ctrl Pts',(-30.9757663112028,0.966231982727323,
305.875321979995));
#17751=CARTESIAN_POINT('Ctrl Pts',(-30.9465559771828,0.877704110886948,
305.870276676176));
#17752=CARTESIAN_POINT('Ctrl Pts',(-30.9215909612622,0.787889143159898,
305.865231372356));
#17753=CARTESIAN_POINT('Ctrl Pts',(-30.8966526629464,0.698170295572656,
305.86019146803));
#17754=CARTESIAN_POINT('Ctrl Pts',(-30.8759507704791,0.60716751572271,305.855151563704));
#17755=CARTESIAN_POINT('Ctrl Pts',(-30.8596096412037,0.515316450226135,
305.850111659378));
#17756=CARTESIAN_POINT('Ctrl Pts',(-30.8432802910977,0.423531593694662,
305.845075387964));
#17757=CARTESIAN_POINT('Ctrl Pts',(-30.8313055338947,0.330900103028787,
305.840039116549));
#17758=CARTESIAN_POINT('Ctrl Pts',(-30.8237590265882,0.237869544876798,
305.835002845135));
#17759=CARTESIAN_POINT('Ctrl Pts',(-30.8162152633626,0.144872814741193,
305.829968405024));
#17760=CARTESIAN_POINT('Ctrl Pts',(-30.8130965870602,0.05147774775249,305.824933964912));
#17761=CARTESIAN_POINT('Ctrl Pts',(-30.8144248730321,-0.0418622454265086,
305.8198995248));
#17762=CARTESIAN_POINT('Ctrl Pts',(-30.8157530475937,-0.135194409683775,
305.814865506953));
#17763=CARTESIAN_POINT('Ctrl Pts',(-30.8215274363334,-0.228471065105655,
305.809831489107));
#17764=CARTESIAN_POINT('Ctrl Pts',(-30.8317177925861,-0.321239225290878,
305.80479747126));
#17765=CARTESIAN_POINT('Ctrl Pts',(-30.8419101448092,-0.414025555842328,
305.799762467408));
#17766=CARTESIAN_POINT('Ctrl Pts',(-30.8565201334637,-0.50630275182035,
305.794727463556));
#17767=CARTESIAN_POINT('Ctrl Pts',(-30.8754658266925,-0.597624513454089,
305.789692459703));
#17768=CARTESIAN_POINT('Ctrl Pts',(-30.8944323377595,-0.689046620936459,
305.784651923306));
#17769=CARTESIAN_POINT('Ctrl Pts',(-30.9177439728114,-0.77951076278748,
305.779611386909));
#17770=CARTESIAN_POINT('Ctrl Pts',(-30.9452680589654,-0.868582679780679,
305.774570850512));
#17771=CARTESIAN_POINT('Ctrl Pts',(-30.9728090557022,-0.957709321861172,
305.769527217249));
#17772=CARTESIAN_POINT('Ctrl Pts',(-31.0045675048311,-1.04544161878498,
305.764483583985));
#17773=CARTESIAN_POINT('Ctrl Pts',(-31.0403621743289,-1.1313643420492,305.759439950722));
#17774=CARTESIAN_POINT('Ctrl Pts',(-31.0762148040231,-1.21742619490936,
305.754388150601));
#17775=CARTESIAN_POINT('Ctrl Pts',(-31.11611651171,-1.3016722234562,305.74933635048));
#17776=CARTESIAN_POINT('Ctrl Pts',(-31.1598397286161,-1.38371105123071,
305.744284550359));
#17777=CARTESIAN_POINT('Ctrl Pts',(-31.1819726503707,-1.42523953619727,
305.741727302638));
#17778=CARTESIAN_POINT('Ctrl Pts',(-31.2050841090988,-1.46620288694025,
305.739170054917));
#17779=CARTESIAN_POINT('Ctrl Pts',(-31.229140462597,-1.50655332203433,305.736612807196));
#17780=CARTESIAN_POINT('Ctrl Pts',(-31.2766679332513,-1.58627255795134,
305.731560523772));
#17781=CARTESIAN_POINT('Ctrl Pts',(-31.328056785282,-1.66388364639719,305.726508240347));
#17782=CARTESIAN_POINT('Ctrl Pts',(-31.3830945186209,-1.73898841929601,
305.721455956923));
#17783=CARTESIAN_POINT('Ctrl Pts',(-31.4380563444698,-1.81398960844497,
305.716410641558));
#17784=CARTESIAN_POINT('Ctrl Pts',(-31.4966567910936,-1.88649099569085,
305.711365326192));
#17785=CARTESIAN_POINT('Ctrl Pts',(-31.5586384584447,-1.9561206503502,305.706320010826));
#17786=CARTESIAN_POINT('Ctrl Pts',(-31.6205537925266,-2.02567578680408,
305.701280094997));
#17787=CARTESIAN_POINT('Ctrl Pts',(-31.6858428610082,-2.0923649693723,305.696240179168));
#17788=CARTESIAN_POINT('Ctrl Pts',(-31.7542067899118,-2.1558477152417,305.691200263339));
#17789=CARTESIAN_POINT('Ctrl Pts',(-31.8225214386815,-2.21928469957774,
305.686163980532));
#17790=CARTESIAN_POINT('Ctrl Pts',(-31.8939062176371,-2.27951953993609,
305.681127697726));
#17791=CARTESIAN_POINT('Ctrl Pts',(-31.9680247735594,-2.33624791866612,
305.67609141492));
#17792=CARTESIAN_POINT('Ctrl Pts',(-32.0421163772862,-2.39295566889988,
305.671056963489));
#17793=CARTESIAN_POINT('Ctrl Pts',(-32.1189394306651,-2.44615922084135,
305.666022512058));
#17794=CARTESIAN_POINT('Ctrl Pts',(-32.1981246233513,-2.49559462165916,
305.660988060626));
#17795=CARTESIAN_POINT('Ctrl Pts',(-32.2773031730102,-2.54502587522794,
305.655954031547));
#17796=CARTESIAN_POINT('Ctrl Pts',(-32.3588430910346,-2.59068937108095,
305.650920002467));
#17797=CARTESIAN_POINT('Ctrl Pts',(-32.4423471949681,-2.63236520215651,
305.645885973388));
#17798=CARTESIAN_POINT('Ctrl Pts',(-32.5258676530354,-2.67404919537122,
305.640850958403));
#17799=CARTESIAN_POINT('Ctrl Pts',(-32.6113526633519,-2.71174377474132,
305.635815943417));
#17800=CARTESIAN_POINT('Ctrl Pts',(-32.6983826723174,-2.74527610338617,
305.630780928432));
#17801=CARTESIAN_POINT('Ctrl Pts',(-32.7855083072953,-2.7788452763668,305.62574038112));
#17802=CARTESIAN_POINT('Ctrl Pts',(-32.8741819143405,-2.80824290968469,
305.620699833809));
#17803=CARTESIAN_POINT('Ctrl Pts',(-32.9639665807851,-2.83334534256119,
305.615659286497));
#17804=CARTESIAN_POINT('Ctrl Pts',(-33.0538064081832,-2.85846319760482,
305.610615642427));
#17805=CARTESIAN_POINT('Ctrl Pts',(-33.1447582211694,-2.87928049974766,
305.605571998358));
#17806=CARTESIAN_POINT('Ctrl Pts',(-33.2363748058769,-2.89572471593017,
305.600528354288));
#17807=CARTESIAN_POINT('Ctrl Pts',(-33.3281397346472,-2.91219555831628,
305.595476543633));
#17808=CARTESIAN_POINT('Ctrl Pts',(-33.4205711440586,-2.92427912122125,
305.590424732978));
#17809=CARTESIAN_POINT('Ctrl Pts',(-33.5132167756848,-2.93195474225857,
305.585372922323));
#17810=CARTESIAN_POINT('Ctrl Pts',(-33.5601123294462,-2.93584000368633,
305.582815786557));
#17811=CARTESIAN_POINT('Ctrl Pts',(-33.6070627676053,-2.93859669249374,
305.580258650791));
#17812=CARTESIAN_POINT('Ctrl Pts',(-33.6540097105623,-2.94022721129498,
305.577701515026));
#17813=CARTESIAN_POINT('Ctrl Pts',(-33.746765573912,-2.94344872412606,305.572649230027));
#17814=CARTESIAN_POINT('Ctrl Pts',(-33.8398405204643,-2.9422824371313,305.567596945028));
#17815=CARTESIAN_POINT('Ctrl Pts',(-33.9327847446478,-2.93669134404347,
305.562544660029));
#17816=CARTESIAN_POINT('Ctrl Pts',(-34.025600783513,-2.93110796198938,305.557499342959));
#17817=CARTESIAN_POINT('Ctrl Pts',(-34.1182860186593,-2.92111192679462,
305.552454025889));
#17818=CARTESIAN_POINT('Ctrl Pts',(-34.2103883835416,-2.90671818695414,
305.54740870882));
#17819=CARTESIAN_POINT('Ctrl Pts',(-34.3023921820682,-2.89233985104474,
305.542368791161));
#17820=CARTESIAN_POINT('Ctrl Pts',(-34.3938139136144,-2.87357323329236,
305.537328873502));
#17821=CARTESIAN_POINT('Ctrl Pts',(-34.4842054863197,-2.8504851787963,305.532288955843));
#17822=CARTESIAN_POINT('Ctrl Pts',(-34.5745319034569,-2.82741376650773,
305.52725267103));
#17823=CARTESIAN_POINT('Ctrl Pts',(-34.6638292084842,-2.8000272185105,305.522216386218));
#17824=CARTESIAN_POINT('Ctrl Pts',(-34.7516594132438,-2.76844347323014,
305.517180101405));
#17825=CARTESIAN_POINT('Ctrl Pts',(-34.8394576816598,-2.73687121226023,
305.512145647859));
#17826=CARTESIAN_POINT('Ctrl Pts',(-34.9257894919556,-2.70110493606891,
305.507111194314));
#17827=CARTESIAN_POINT('Ctrl Pts',(-35.0102329392263,-2.66131214940086,
305.502076740768));
#17828=CARTESIAN_POINT('Ctrl Pts',(-35.0946693041096,-2.62152270020831,
305.497042709468));
#17829=CARTESIAN_POINT('Ctrl Pts',(-35.1772172190718,-2.57770760152444,
305.492008678169));
#17830=CARTESIAN_POINT('Ctrl Pts',(-35.2574767108073,-2.53008164328739,
305.48697464687));
#17831=CARTESIAN_POINT('Ctrl Pts',(-35.3377519228428,-2.48244635662909,
305.481939629562));
#17832=CARTESIAN_POINT('Ctrl Pts',(-35.4157374396239,-2.43099895502573,
305.476904612255));
#17833=CARTESIAN_POINT('Ctrl Pts',(-35.4910607411503,-2.37599852724254,
305.471869594948));
#17834=CARTESIAN_POINT('Ctrl Pts',(-35.5664668077397,-2.32093766512127,
305.466829045176));
#17835=CARTESIAN_POINT('Ctrl Pts',(-35.6392044606158,-2.2623162462482,305.461788495404));
#17836=CARTESIAN_POINT('Ctrl Pts',(-35.7089331178811,-2.20043458539732,
305.456747945632));
#17837=CARTESIAN_POINT('Ctrl Pts',(-35.7787046154201,-2.13851490535329,
305.451704299019));
#17838=CARTESIAN_POINT('Ctrl Pts',(-35.8454631193548,-2.07333130579444,
305.446660652407));
#17839=CARTESIAN_POINT('Ctrl Pts',(-35.9089054489725,-2.00522045131894,
305.441617005794));
#17840=CARTESIAN_POINT('Ctrl Pts',(-35.9724505045914,-1.93699931155341,
305.436565192495));
#17841=CARTESIAN_POINT('Ctrl Pts',(-36.032668379603,-1.86584179309872,305.431513379195));
#17842=CARTESIAN_POINT('Ctrl Pts',(-36.0892967659652,-1.79211689380081,
305.426461565895));
#17843=CARTESIAN_POINT('Ctrl Pts',(-36.1179607823449,-1.75479900683956,
305.423904451549));
#17844=CARTESIAN_POINT('Ctrl Pts',(-36.1457058122861,-1.71682376995429,
305.421347337203));
#17845=CARTESIAN_POINT('Ctrl Pts',(-36.1725022585399,-1.67824155948422,
305.418790222857));
#17846=CARTESIAN_POINT('Ctrl Pts',(-36.226108056709,-1.60105855664165,305.413674762611));
#17847=CARTESIAN_POINT('Ctrl Pts',(-36.2761046912628,-1.52117167573944,
305.408559302366));
#17848=CARTESIAN_POINT('Ctrl Pts',(-36.3222123092792,-1.43894764155196,
305.40344384212));
#17849=CARTESIAN_POINT('Ctrl Pts',(-36.3682523754555,-1.35684407302804,
305.398335876487));
#17850=CARTESIAN_POINT('Ctrl Pts',(-36.4104145423665,-1.27241052870167,
305.393227910855));
#17851=CARTESIAN_POINT('Ctrl Pts',(-36.4484613602111,-1.18604377188642,
305.388119945222));
#17852=CARTESIAN_POINT('Ctrl Pts',(-36.4864621471144,-1.09978150588898,
305.383018159461));
#17853=CARTESIAN_POINT('Ctrl Pts',(-36.5203573121079,-1.01159106855782,
305.377916373701));
#17854=CARTESIAN_POINT('Ctrl Pts',(-36.5499550823211,-0.921894130345155,
305.37281458794));
#17855=CARTESIAN_POINT('Ctrl Pts',(-36.5795207165609,-0.832294581172113,
305.367718341477));
#17856=CARTESIAN_POINT('Ctrl Pts',(-36.6047981081081,-0.741192193038616,
305.362622095014));
#17857=CARTESIAN_POINT('Ctrl Pts',(-36.6256438502739,-0.649027881487562,
305.357525848551));
#17858=CARTESIAN_POINT('Ctrl Pts',(-36.6464764407366,-0.556921716950648,
305.35243281734));
#17859=CARTESIAN_POINT('Ctrl Pts',(-36.6628828474354,-0.463755379522535,
305.347339786129));
#17860=CARTESIAN_POINT('Ctrl Pts',(-36.6747698928038,-0.369983528987202,
305.342246754918));
#17861=CARTESIAN_POINT('Ctrl Pts',(-36.686652822147,-0.276244148025949,
305.337155487227));
#17862=CARTESIAN_POINT('Ctrl Pts',(-36.6940194483778,-0.181900096871285,
305.332064219537));
#17863=CARTESIAN_POINT('Ctrl Pts',(-36.6968281006551,-0.0874138727897526,
305.326972951846));
#17864=CARTESIAN_POINT('Ctrl Pts',(-36.6977101757216,-0.0577398746709374,
305.325374006927));
#17865=CARTESIAN_POINT('Ctrl Pts',(-36.6981430762226,-0.0280518897877842,
305.323775062009));
#17866=CARTESIAN_POINT('Ctrl Pts',(-36.6981265705531,0.00163568983778872,
305.32217611709));
#17867=CARTESIAN_POINT('',(-36.6981264963869,0.00176405078021327,304.322176117128));
#17868=CARTESIAN_POINT('Ctrl Pts',(-36.6981265705527,0.00163569045731642,
305.322176117057));
#17869=CARTESIAN_POINT('Ctrl Pts',(-36.6980687822406,0.105575398122983,
305.316578022853));
#17870=CARTESIAN_POINT('Ctrl Pts',(-36.6924986516524,0.20931837606196,305.310979928649));
#17871=CARTESIAN_POINT('Ctrl Pts',(-36.6815031459867,0.312311626854009,
305.305381834446));
#17872=CARTESIAN_POINT('Ctrl Pts',(-36.6704676688315,0.415679284586532,
305.299763389731));
#17873=CARTESIAN_POINT('Ctrl Pts',(-36.6539674239736,0.518291508928275,
305.294144945016));
#17874=CARTESIAN_POINT('Ctrl Pts',(-36.6321402925598,0.619606073486603,
305.288526500301));
#17875=CARTESIAN_POINT('Ctrl Pts',(-36.6102032420979,0.721430847119007,
305.282879761712));
#17876=CARTESIAN_POINT('Ctrl Pts',(-36.5828856408373,0.821944618092324,
305.277233023124));
#17877=CARTESIAN_POINT('Ctrl Pts',(-36.5503759963964,0.920617557561025,
305.271586284535));
#17878=CARTESIAN_POINT('Ctrl Pts',(-36.52790863729,0.988810255551313,305.267683833253));
#17879=CARTESIAN_POINT('Ctrl Pts',(-36.5029624841091,1.0561241721974,305.26378138197));
#17880=CARTESIAN_POINT('Ctrl Pts',(-36.4756127117875,1.12239101954654,305.259878930687));
#17881=CARTESIAN_POINT('Ctrl Pts',(-36.4402040385224,1.20818409740135,305.254826580679));
#17882=CARTESIAN_POINT('Ctrl Pts',(-36.4006679936895,1.29245392580459,305.249774230672));
#17883=CARTESIAN_POINT('Ctrl Pts',(-36.3571568190445,1.37477562235905,305.244721880664));
#17884=CARTESIAN_POINT('Ctrl Pts',(-36.3137056557643,1.45698377940559,305.239676498945));
#17885=CARTESIAN_POINT('Ctrl Pts',(-36.2662904630271,1.53724875446474,305.234631117226));
#17886=CARTESIAN_POINT('Ctrl Pts',(-36.2151117253316,1.61516508283266,305.229585735506));
#17887=CARTESIAN_POINT('Ctrl Pts',(-36.1639877620064,1.69299802075333,305.224545753639));
#17888=CARTESIAN_POINT('Ctrl Pts',(-36.1091085024822,1.76848693894027,305.219505771772));
#17889=CARTESIAN_POINT('Ctrl Pts',(-36.0507200434947,1.84125144416985,305.214465789905));
#17890=CARTESIAN_POINT('Ctrl Pts',(-35.9923736818115,1.91396348715653,305.209429441798));
#17891=CARTESIAN_POINT('Ctrl Pts',(-35.9305234268017,1.98395467595569,305.204393093691));
#17892=CARTESIAN_POINT('Ctrl Pts',(-35.8654577225004,2.05087493759837,305.199356745583));
#17893=CARTESIAN_POINT('Ctrl Pts',(-35.80041568435,2.11777085853768,305.194322229332));
#17894=CARTESIAN_POINT('Ctrl Pts',(-35.7321608297071,2.18159775313175,305.18928771308));
#17895=CARTESIAN_POINT('Ctrl Pts',(-35.6610200879099,2.24204068202593,305.184253196829));
#17896=CARTESIAN_POINT('Ctrl Pts',(-35.5898853220741,2.30247853359578,305.179219103487));
#17897=CARTESIAN_POINT('Ctrl Pts',(-35.5158654897394,2.35953269714093,305.174185010144));
#17898=CARTESIAN_POINT('Ctrl Pts',(-35.439321511082,2.4129277492064,305.169150916802));
#17899=CARTESIAN_POINT('Ctrl Pts',(-35.3627625512686,2.46633325172957,305.164115838189));
#17900=CARTESIAN_POINT('Ctrl Pts',(-35.28367882854,2.51607796663302,305.159080759576));
#17901=CARTESIAN_POINT('Ctrl Pts',(-35.202460252322,2.5619297797343,305.154045680963));
#17902=CARTESIAN_POINT('Ctrl Pts',(-35.1211524583318,2.60783196058155,305.149005071368));
#17903=CARTESIAN_POINT('Ctrl Pts',(-35.0377055171747,2.64983248486244,305.143964461773));
#17904=CARTESIAN_POINT('Ctrl Pts',(-34.952533675687,2.68774536122904,305.138923852178));
#17905=CARTESIAN_POINT('Ctrl Pts',(-34.8673095192103,2.72568152477222,305.133880146495));
#17906=CARTESIAN_POINT('Ctrl Pts',(-34.7803587668598,2.7595248809654,305.128836440813));
#17907=CARTESIAN_POINT('Ctrl Pts',(-34.6921133049353,2.78913852009093,305.123792735131));
#17908=CARTESIAN_POINT('Ctrl Pts',(-34.6037249878439,2.81880009892089,305.118740864503));
#17909=CARTESIAN_POINT('Ctrl Pts',(-34.5140382037932,2.84421817004464,305.113688993875));
#17910=CARTESIAN_POINT('Ctrl Pts',(-34.4234973861619,2.86530640619576,305.108637123247));
#17911=CARTESIAN_POINT('Ctrl Pts',(-34.3776792810693,2.87597809047547,305.106080628337));
#17912=CARTESIAN_POINT('Ctrl Pts',(-34.3316425948253,2.88554178733248,305.103524133428));
#17913=CARTESIAN_POINT('Ctrl Pts',(-34.2854453897896,2.89399137334049,305.100967638519));
#17914=CARTESIAN_POINT('Ctrl Pts',(-34.1941472619466,2.91069003255554,305.095915315573));
#17915=CARTESIAN_POINT('Ctrl Pts',(-34.1018943172055,2.92309408399761,305.090862992627));
#17916=CARTESIAN_POINT('Ctrl Pts',(-34.0091261817993,2.9311014016559,305.08581066968));
#17917=CARTESIAN_POINT('Ctrl Pts',(-33.9164859724032,2.93909767733092,305.080765313819));
#17918=CARTESIAN_POINT('Ctrl Pts',(-33.8233324228397,2.94270922938106,305.075719957959));
#17919=CARTESIAN_POINT('Ctrl Pts',(-33.7301149631016,2.94188500329676,305.070674602098));
#17920=CARTESIAN_POINT('Ctrl Pts',(-33.6369972479132,2.94106165915089,305.065634644869));
#17921=CARTESIAN_POINT('Ctrl Pts',(-33.543816200319,2.93581197491237,305.06059468764));
#17922=CARTESIAN_POINT('Ctrl Pts',(-33.4510248765455,2.92613681820438,305.055554730411));
#17923=CARTESIAN_POINT('Ctrl Pts',(-33.3583004195325,2.91646863355327,305.050518405047));
#17924=CARTESIAN_POINT('Ctrl Pts',(-33.2659655687111,2.90238136107195,305.045482079684));
#17925=CARTESIAN_POINT('Ctrl Pts',(-33.1744708260699,2.88392788847893,305.04044575432));
#17926=CARTESIAN_POINT('Ctrl Pts',(-33.0830093412368,2.86548112361612,305.035411259632));
#17927=CARTESIAN_POINT('Ctrl Pts',(-32.9923877929635,2.84267139930572,305.030376764943));
#17928=CARTESIAN_POINT('Ctrl Pts',(-32.9030479908327,2.8156029835587,305.025342270255));
#17929=CARTESIAN_POINT('Ctrl Pts',(-32.8137156721683,2.78853683517266,305.020308197276));
#17930=CARTESIAN_POINT('Ctrl Pts',(-32.725665311288,2.75721283359567,305.015274124297));
#17931=CARTESIAN_POINT('Ctrl Pts',(-32.6393239072545,2.72178522216918,305.010240051319));
#17932=CARTESIAN_POINT('Ctrl Pts',(-32.5529655835358,2.68635066825618,305.00520499185));
#17933=CARTESIAN_POINT('Ctrl Pts',(-32.4683172925889,2.64681107641035,305.000169932382));
#17934=CARTESIAN_POINT('Ctrl Pts',(-32.385785325272,2.6033685150744,304.995134872913));
#17935=CARTESIAN_POINT('Ctrl Pts',(-32.3031626651733,2.55987821554846,304.990094280515));
#17936=CARTESIAN_POINT('Ctrl Pts',(-32.2226613645728,2.51247659262798,304.985053688117));
#17937=CARTESIAN_POINT('Ctrl Pts',(-32.1446621217005,2.46141115309973,304.980013095719));
#17938=CARTESIAN_POINT('Ctrl Pts',(-32.0666149525732,2.41031433666084,304.974969406153));
#17939=CARTESIAN_POINT('Ctrl Pts',(-31.9910732611988,2.35554948244164,304.969925716588));
#17940=CARTESIAN_POINT('Ctrl Pts',(-31.9183860381808,2.29740550717932,304.964882027022));
#17941=CARTESIAN_POINT('Ctrl Pts',(-31.8455811196529,2.23916738490559,304.95983017069));
#17942=CARTESIAN_POINT('Ctrl Pts',(-31.7756402295717,2.1775395117591,304.954778314357));
#17943=CARTESIAN_POINT('Ctrl Pts',(-31.7088766314584,2.11284874638222,304.949726458025));
#17944=CARTESIAN_POINT('Ctrl Pts',(-31.6750881109795,2.08010926989354,304.947169754133));
#17945=CARTESIAN_POINT('Ctrl Pts',(-31.6421127640942,2.04658584750536,304.944613050241));
#17946=CARTESIAN_POINT('Ctrl Pts',(-31.6099871925103,2.01232398442582,304.942056346349));
#17947=CARTESIAN_POINT('Ctrl Pts',(-31.546509622489,1.94462527260648,304.937004503149));
#17948=CARTESIAN_POINT('Ctrl Pts',(-31.4861244092015,1.8737984283578,304.93195265995));
#17949=CARTESIAN_POINT('Ctrl Pts',(-31.4291554856856,1.80015761921618,304.92690081675));
#17950=CARTESIAN_POINT('Ctrl Pts',(-31.3722651506293,1.72661839735042,304.921855942554));
#17951=CARTESIAN_POINT('Ctrl Pts',(-31.3187820100551,1.65027327269262,304.916811068357));
#17952=CARTESIAN_POINT('Ctrl Pts',(-31.2689923786189,1.57147231903376,304.91176619416));
#17953=CARTESIAN_POINT('Ctrl Pts',(-31.2192560404307,1.49275571142532,304.906726719837));
#17954=CARTESIAN_POINT('Ctrl Pts',(-31.1732055894753,1.41158887323433,304.901687245514));
#17955=CARTESIAN_POINT('Ctrl Pts',(-31.1310856598489,1.32835305167465,304.896647771191));
#17956=CARTESIAN_POINT('Ctrl Pts',(-31.0889960839191,1.2451772139491,304.891611928562));
#17957=CARTESIAN_POINT('Ctrl Pts',(-31.0508315993594,1.15993575175802,304.886576085933));
#17958=CARTESIAN_POINT('Ctrl Pts',(-31.0167917289375,1.07303594270398,304.881540243303));
#17959=CARTESIAN_POINT('Ctrl Pts',(-30.9827642310606,0.986167719310951,
304.876506231062));
#17960=CARTESIAN_POINT('Ctrl Pts',(-30.9528585309551,0.897642759815976,
304.871472218822));
#17961=CARTESIAN_POINT('Ctrl Pts',(-30.9272262524522,0.807888864647229,
304.866438206581));
#17962=CARTESIAN_POINT('Ctrl Pts',(-30.9015961167322,0.718142472639308,
304.861404615168));
#17963=CARTESIAN_POINT('Ctrl Pts',(-30.8802388141739,0.627167776529021,
304.856371023756));
#17964=CARTESIAN_POINT('Ctrl Pts',(-30.8632559364977,0.535407194401948,
304.851337432344));
#17965=CARTESIAN_POINT('Ctrl Pts',(-30.8462697255113,0.443628601988464,
304.846302852965));
#17966=CARTESIAN_POINT('Ctrl Pts',(-30.833659725059,0.351064254181437,304.841268273586));
#17967=CARTESIAN_POINT('Ctrl Pts',(-30.8254761077667,0.258165063107938,
304.836233694206));
#17968=CARTESIAN_POINT('Ctrl Pts',(-30.8172834884007,0.165163681850032,
304.831193576732));
#17969=CARTESIAN_POINT('Ctrl Pts',(-30.8135270104799,0.071827165406105,
304.826153459257));
#17970=CARTESIAN_POINT('Ctrl Pts',(-30.8142047884544,-0.0213904792602384,
304.821113341782));
#17971=CARTESIAN_POINT('Ctrl Pts',(-30.8148829832253,-0.114665447679882,
304.816070124911));
#17972=CARTESIAN_POINT('Ctrl Pts',(-30.820000838066,-0.207820955455111,
304.81102690804));
#17973=CARTESIAN_POINT('Ctrl Pts',(-30.8295044839954,-0.300407225238978,
304.805983691168));
#17974=CARTESIAN_POINT('Ctrl Pts',(-30.8390235349569,-0.393143573684762,
304.800932299443));
#17975=CARTESIAN_POINT('Ctrl Pts',(-30.8529425033414,-0.485308403255275,
304.795880907718));
#17976=CARTESIAN_POINT('Ctrl Pts',(-30.8711562754231,-0.576461423340376,
304.790829515992));
#17977=CARTESIAN_POINT('Ctrl Pts',(-30.880392214324,-0.622683793992275,
304.788268028722));
#17978=CARTESIAN_POINT('Ctrl Pts',(-30.8907316985239,-0.668646219021566,
304.785706541451));
#17979=CARTESIAN_POINT('Ctrl Pts',(-30.90215618544,-0.714292968935603,304.78314505418));
#17980=CARTESIAN_POINT('Ctrl Pts',(-30.9246933650259,-0.804340689054872,
304.77809198711));
#17981=CARTESIAN_POINT('Ctrl Pts',(-30.9515368623356,-0.893482143182679,
304.77303892004));
#17982=CARTESIAN_POINT('Ctrl Pts',(-30.982597877132,-0.981274714082561,
304.76798585297));
#17983=CARTESIAN_POINT('Ctrl Pts',(-31.0136160475477,-1.06894618725381,
304.762939755908));
#17984=CARTESIAN_POINT('Ctrl Pts',(-31.0488400284389,-1.15527205942261,
304.757893658847));
#17985=CARTESIAN_POINT('Ctrl Pts',(-31.0881304644289,-1.2398219030998,304.752847561785));
#17986=CARTESIAN_POINT('Ctrl Pts',(-31.1273788348419,-1.32428122505439,
304.747806867233));
#17987=CARTESIAN_POINT('Ctrl Pts',(-31.1706848205516,-1.40696789742434,
304.742766172682));
#17988=CARTESIAN_POINT('Ctrl Pts',(-31.2178602900946,-1.487469657225,304.73772547813));
#17989=CARTESIAN_POINT('Ctrl Pts',(-31.2650016873628,-1.56791327498474,
304.732688424198));
#17990=CARTESIAN_POINT('Ctrl Pts',(-31.3160067895996,-1.64617473474176,
304.727651370266));
#17991=CARTESIAN_POINT('Ctrl Pts',(-31.3706411549913,-1.72186560531297,
304.722614316334));
#17992=CARTESIAN_POINT('Ctrl Pts',(-31.4252556022491,-1.79752888114809,
304.717579098768));
#17993=CARTESIAN_POINT('Ctrl Pts',(-31.4834964244442,-1.87062306985752,
304.712543881203));
#17994=CARTESIAN_POINT('Ctrl Pts',(-31.5450859880084,-1.94078889413562,
304.707508663637));
#17995=CARTESIAN_POINT('Ctrl Pts',(-31.6066703131885,-2.01094875059188,
304.702473874332));
#17996=CARTESIAN_POINT('Ctrl Pts',(-31.671602520337,-2.07818040417835,304.697439085027));
#17997=CARTESIAN_POINT('Ctrl Pts',(-31.739565591196,-2.14215872022952,304.692404295722));
#17998=CARTESIAN_POINT('Ctrl Pts',(-31.8075418782633,-2.20614947760719,
304.687368527345));
#17999=CARTESIAN_POINT('Ctrl Pts',(-31.8785498759646,-2.26688533688328,
304.682332758967));
#18000=CARTESIAN_POINT('Ctrl Pts',(-31.9522375755747,-2.32407978635046,
304.677296990589));
#18001=CARTESIAN_POINT('Ctrl Pts',(-32.0260060111398,-2.38133690093709,
304.672255704769));
#18002=CARTESIAN_POINT('Ctrl Pts',(-32.1024596578963,-2.4350445877322,304.66721441895));
#18003=CARTESIAN_POINT('Ctrl Pts',(-32.1812157087587,-2.48495841920214,
304.66217313313));
#18004=CARTESIAN_POINT('Ctrl Pts',(-32.2600200228257,-2.53490283881662,
304.657128757915));
#18005=CARTESIAN_POINT('Ctrl Pts',(-32.341129164255,-2.58104855506556,304.6520843827));
#18006=CARTESIAN_POINT('Ctrl Pts',(-32.4241357195483,-2.62319712593525,
304.647040007484));
#18007=CARTESIAN_POINT('Ctrl Pts',(-32.5072763533554,-2.66541377838859,
304.64198748421));
#18008=CARTESIAN_POINT('Ctrl Pts',(-32.5923201150392,-2.70362021404384,
304.636934960935));
#18009=CARTESIAN_POINT('Ctrl Pts',(-32.6788398043432,-2.73766620384124,
304.631882437661));
#18010=CARTESIAN_POINT('Ctrl Pts',(-32.7224985866249,-2.75484618296607,
304.629332879111));
#18011=CARTESIAN_POINT('Ctrl Pts',(-32.7665329455022,-2.77096757030336,
304.626783320561));
#18012=CARTESIAN_POINT('Ctrl Pts',(-32.8108867998765,-2.78601595765738,
304.624233762011));
#18013=CARTESIAN_POINT('Ctrl Pts',(-32.8987820482044,-2.8158370805806,304.619181346949));
#18014=CARTESIAN_POINT('Ctrl Pts',(-32.9882474431162,-2.84154809940506,
304.614128931887));
#18015=CARTESIAN_POINT('Ctrl Pts',(-33.0788628772053,-2.86298398070318,
304.609076516826));
#18016=CARTESIAN_POINT('Ctrl Pts',(-33.1693534986685,-2.88439033647221,
304.604031060901));
#18017=CARTESIAN_POINT('Ctrl Pts',(-33.260990583047,-2.90153315461889,304.598985604975));
#18018=CARTESIAN_POINT('Ctrl Pts',(-33.3533368915402,-2.91429650313414,
304.59394014905));
#18019=CARTESIAN_POINT('Ctrl Pts',(-33.4455845304219,-2.92704621434587,
304.588900084063));
#18020=CARTESIAN_POINT('Ctrl Pts',(-33.5385394495211,-2.93542569637416,
304.583860019075));
#18021=CARTESIAN_POINT('Ctrl Pts',(-33.631753266253,-2.93936985901248,304.578819954088));
#18022=CARTESIAN_POINT('Ctrl Pts',(-33.72490011394,-2.943311187985,304.573783510112));
#18023=CARTESIAN_POINT('Ctrl Pts',(-33.8183050470046,-2.94282351250116,
304.568747066137));
#18024=CARTESIAN_POINT('Ctrl Pts',(-33.9115146381822,-2.93789358039899,
304.563710622161));
#18025=CARTESIAN_POINT('Ctrl Pts',(-34.0046904724401,-2.93296543372813,
304.558676002191));
#18026=CARTESIAN_POINT('Ctrl Pts',(-34.0976706622015,-2.92359824996414,
304.553641382221));
#18027=CARTESIAN_POINT('Ctrl Pts',(-34.1900029021185,-2.90983087540809,
304.548606762251));
#18028=CARTESIAN_POINT('Ctrl Pts',(-34.2823275267241,-2.89606463634755,
304.543572557523));
#18029=CARTESIAN_POINT('Ctrl Pts',(-34.3740038684061,-2.87789899375566,
304.538538352795));
#18030=CARTESIAN_POINT('Ctrl Pts',(-34.4645870007847,-2.85542439281381,
304.533504148067));
#18031=CARTESIAN_POINT('Ctrl Pts',(-34.5551879964678,-2.83294535980355,
304.528468950577));
#18032=CARTESIAN_POINT('Ctrl Pts',(-34.6446949236627,-2.80615578816217,
304.523433753086));
#18033=CARTESIAN_POINT('Ctrl Pts',(-34.7326763824026,-2.77519645305691,
304.518398555595));
#18034=CARTESIAN_POINT('Ctrl Pts',(-34.8207546691694,-2.74420304564398,
304.513357816616));
#18035=CARTESIAN_POINT('Ctrl Pts',(-34.9073037166122,-2.70903086219687,
304.508317077637));
#18036=CARTESIAN_POINT('Ctrl Pts',(-34.9919108299709,-2.66986935785409,
304.503276338658));
#18037=CARTESIAN_POINT('Ctrl Pts',(-35.0765700134753,-2.63068375216623,
304.498232497434));
#18038=CARTESIAN_POINT('Ctrl Pts',(-35.1592844901276,-2.5875041432499,304.49318865621));
#18039=CARTESIAN_POINT('Ctrl Pts',(-35.2396669071173,-2.54056557068138,
304.488144814986));
#18040=CARTESIAN_POINT('Ctrl Pts',(-35.3201795764497,-2.4935509384562,304.483092800679));
#18041=CARTESIAN_POINT('Ctrl Pts',(-35.3983522699958,-2.44276542423807,
304.478040786372));
#18042=CARTESIAN_POINT('Ctrl Pts',(-35.4738274576828,-2.38848680642084,
304.472988772065));
#18043=CARTESIAN_POINT('Ctrl Pts',(-35.512004678629,-2.36103133597326,304.47043333799));
#18044=CARTESIAN_POINT('Ctrl Pts',(-35.5494922554282,-2.33268275877039,
304.467877903916));
#18045=CARTESIAN_POINT('Ctrl Pts',(-35.586247416328,-2.30348070410589,304.465322469841));
#18046=CARTESIAN_POINT('Ctrl Pts',(-35.6579640035599,-2.24650172076255,
304.460336312625));
#18047=CARTESIAN_POINT('Ctrl Pts',(-35.7271624638713,-2.18605451410487,
304.455350155409));
#18048=CARTESIAN_POINT('Ctrl Pts',(-35.7934814879079,-2.1223927048308,304.450363998194));
#18049=CARTESIAN_POINT('Ctrl Pts',(-35.8597084827952,-2.05881923735966,
304.445384760136));
#18050=CARTESIAN_POINT('Ctrl Pts',(-35.9230636498218,-1.99204033925046,
304.440405522078));
#18051=CARTESIAN_POINT('Ctrl Pts',(-35.9832171786362,-1.92235102120401,
304.43542628402));
#18052=CARTESIAN_POINT('Ctrl Pts',(-36.0433021744706,-1.85274110027249,
304.430452718814));
#18053=CARTESIAN_POINT('Ctrl Pts',(-36.1001924846239,-1.7802276933431,304.425479153607));
#18054=CARTESIAN_POINT('Ctrl Pts',(-36.1535947455384,-1.70514296474278,
304.420505588401));
#18055=CARTESIAN_POINT('Ctrl Pts',(-36.2069639779374,-1.63010467494626,
304.415535099271));
#18056=CARTESIAN_POINT('Ctrl Pts',(-36.2568491791805,-1.55249859148548,
304.410564610142));
#18057=CARTESIAN_POINT('Ctrl Pts',(-36.3029975866806,-1.47268949319156,
304.405594121013));
#18058=CARTESIAN_POINT('Ctrl Pts',(-36.3491311627868,-1.39290604432389,
304.400625229323));
#18059=CARTESIAN_POINT('Ctrl Pts',(-36.3915301017078,-1.31092138203121,
304.395656337633));
#18060=CARTESIAN_POINT('Ctrl Pts',(-36.4299859857538,-1.22712764591723,
304.390687445943));
#18061=CARTESIAN_POINT('Ctrl Pts',(-36.4684409351638,-1.14333594633526,
304.385718675017));
#18062=CARTESIAN_POINT('Ctrl Pts',(-36.5029528313446,-1.05773567643545,
304.380749904092));
#18063=CARTESIAN_POINT('Ctrl Pts',(-36.5333606476721,-0.970740648438338,
304.375781133166));
#18064=CARTESIAN_POINT('Ctrl Pts',(-36.563793940195,-0.883672734499373,
304.370808199318));
#18065=CARTESIAN_POINT('Ctrl Pts',(-36.5901161366452,-0.795208161451882,
304.36583526547));
#18066=CARTESIAN_POINT('Ctrl Pts',(-36.6122157250354,-0.705777117085485,
304.360862331623));
#18067=CARTESIAN_POINT('Ctrl Pts',(-36.6343253241258,-0.616305562128438,
304.355887145129));
#18068=CARTESIAN_POINT('Ctrl Pts',(-36.6522084192237,-0.525867112738204,
304.350911958635));
#18069=CARTESIAN_POINT('Ctrl Pts',(-36.6658048340246,-0.43490119471985,
304.345936772141));
#18070=CARTESIAN_POINT('Ctrl Pts',(-36.6794212809244,-0.34380125326306,
304.340954255521));
#18071=CARTESIAN_POINT('Ctrl Pts',(-36.6887383934852,-0.252172746146416,
304.335971738902));
#18072=CARTESIAN_POINT('Ctrl Pts',(-36.693747993094,-0.16045887114041,304.330989222282));
#18073=CARTESIAN_POINT('Ctrl Pts',(-36.6967016629967,-0.106384187850478,
304.328051520564));
#18074=CARTESIAN_POINT('Ctrl Pts',(-36.6981589016092,-0.0522798282133653,
304.325113818846));
#18075=CARTESIAN_POINT('Ctrl Pts',(-36.6981264963869,0.00176405078021291,
304.322176117128));
#18076=CARTESIAN_POINT('',(-32.4661441993221,2.64410822562003,304.000000575692));
#18077=CARTESIAN_POINT('Ctrl Pts',(-36.6981264963864,0.00176405147736488,
304.32217611709));
#18078=CARTESIAN_POINT('Ctrl Pts',(-36.6980685296926,0.098438091249218,
304.316921137284));
#18079=CARTESIAN_POINT('Ctrl Pts',(-36.6932458848664,0.194972500880357,
304.311666157478));
#18080=CARTESIAN_POINT('Ctrl Pts',(-36.6836973150382,0.291026112907725,
304.306411177672));
#18081=CARTESIAN_POINT('Ctrl Pts',(-36.6745022247276,0.383523906099266,
304.30135073252));
#18082=CARTESIAN_POINT('Ctrl Pts',(-36.6609028368121,0.475748978558183,
304.296290287368));
#18083=CARTESIAN_POINT('Ctrl Pts',(-36.6429231820279,0.56724945945851,304.291229842216));
#18084=CARTESIAN_POINT('Ctrl Pts',(-36.6249683274534,0.658623729309089,
304.286176377181));
#18085=CARTESIAN_POINT('Ctrl Pts',(-36.6026452976773,0.749274963134519,
304.281122912146));
#18086=CARTESIAN_POINT('Ctrl Pts',(-36.5760299087034,0.838756059849511,
304.276069447112));
#18087=CARTESIAN_POINT('Ctrl Pts',(-36.5494430792957,0.928141139131874,
304.271021404683));
#18088=CARTESIAN_POINT('Ctrl Pts',(-36.5185731718854,1.01635815514199,304.265973362255));
#18089=CARTESIAN_POINT('Ctrl Pts',(-36.483546892717,1.10297092735386,304.260925319826));
#18090=CARTESIAN_POINT('Ctrl Pts',(-36.4485462929598,1.18952019967226,304.255880978355));
#18091=CARTESIAN_POINT('Ctrl Pts',(-36.4093955445818,1.27446715704452,304.250836636883));
#18092=CARTESIAN_POINT('Ctrl Pts',(-36.3662706263333,1.35739249363027,304.245792295412));
#18093=CARTESIAN_POINT('Ctrl Pts',(-36.3231617525194,1.44028697821212,304.240749830665));
#18094=CARTESIAN_POINT('Ctrl Pts',(-36.276081850531,1.52116094401507,304.235707365919));
#18095=CARTESIAN_POINT('Ctrl Pts',(-36.2252538677438,1.5996176529765,304.230664901173));
#18096=CARTESIAN_POINT('Ctrl Pts',(-36.1744306986924,1.67806693158478,304.22562291398));
#18097=CARTESIAN_POINT('Ctrl Pts',(-36.1198603954981,1.75409903712175,304.220580926787));
#18098=CARTESIAN_POINT('Ctrl Pts',(-36.0618098429471,1.82734527230395,304.215538939594));
#18099=CARTESIAN_POINT('Ctrl Pts',(-36.0037486888104,1.90060488421044,304.2104960316));
#18100=CARTESIAN_POINT('Ctrl Pts',(-35.9422062982593,1.97107726861895,304.205453123605));
#18101=CARTESIAN_POINT('Ctrl Pts',(-35.8774898113599,2.03842682717338,304.20041021561));
#18102=CARTESIAN_POINT('Ctrl Pts',(-35.8127042051563,2.10584831723789,304.195361921627));
#18103=CARTESIAN_POINT('Ctrl Pts',(-35.7447380426834,2.1701400039321,304.190313627643));
#18104=CARTESIAN_POINT('Ctrl Pts',(-35.6739350791312,2.23100342189282,304.185265333659));
#18105=CARTESIAN_POINT('Ctrl Pts',(-35.6030896928956,2.29190330710553,304.180214014913));
#18106=CARTESIAN_POINT('Ctrl Pts',(-35.5294044701116,2.34937056151589,304.175162696166));
#18107=CARTESIAN_POINT('Ctrl Pts',(-35.4532542564075,2.40314859326042,304.170111377419));
#18108=CARTESIAN_POINT('Ctrl Pts',(-35.3769837305676,2.45701159062149,304.165052077934));
#18109=CARTESIAN_POINT('Ctrl Pts',(-35.2982408115342,2.50717349092762,304.159992778449));
#18110=CARTESIAN_POINT('Ctrl Pts',(-35.2174269911309,2.55342248947147,304.154933478964));
#18111=CARTESIAN_POINT('Ctrl Pts',(-35.1778472635012,2.57607359984317,304.152455614477));
#18112=CARTESIAN_POINT('Ctrl Pts',(-35.1377711312594,2.59778684433811,304.14997774999));
#18113=CARTESIAN_POINT('Ctrl Pts',(-35.0972474845098,2.61854156235396,304.147499885503));
#18114=CARTESIAN_POINT('Ctrl Pts',(-35.0155248361917,2.66039689022785,304.142502861191));
#18115=CARTESIAN_POINT('Ctrl Pts',(-34.9316801408628,2.6985049312846,304.137505836878));
#18116=CARTESIAN_POINT('Ctrl Pts',(-34.8460959220293,2.73264190922819,304.132508812566));
#18117=CARTESIAN_POINT('Ctrl Pts',(-34.7606286011108,2.76673226009962,304.127518613597));
#18118=CARTESIAN_POINT('Ctrl Pts',(-34.6734268941707,2.7968621534048,304.122528414629));
#18119=CARTESIAN_POINT('Ctrl Pts',(-34.5848978326186,2.82285368888757,304.11753821566));
#18120=CARTESIAN_POINT('Ctrl Pts',(-34.4964665348272,2.8488165215895,304.112553527431));
#18121=CARTESIAN_POINT('Ctrl Pts',(-34.4067112296767,2.87064995180145,304.107568839202));
#18122=CARTESIAN_POINT('Ctrl Pts',(-34.3160575921275,2.8882246727505,304.102584150973));
#18123=CARTESIAN_POINT('Ctrl Pts',(-34.2254585176852,2.90578881573044,304.097602462956));
#18124=CARTESIAN_POINT('Ctrl Pts',(-34.1339626294416,2.91909925134569,304.092620774938));
#18125=CARTESIAN_POINT('Ctrl Pts',(-34.0420084006083,2.92807715732144,304.087639086921));
#18126=CARTESIAN_POINT('Ctrl Pts',(-33.9500824386787,2.93705230347192,304.082658930284));
#18127=CARTESIAN_POINT('Ctrl Pts',(-33.8576988683455,2.94169752078434,304.077678773646));
#18128=CARTESIAN_POINT('Ctrl Pts',(-33.7653026560057,2.94198569129769,304.072698617009));
#18129=CARTESIAN_POINT('Ctrl Pts',(-33.6729076380417,2.94227385808597,304.067718524749));
#18130=CARTESIAN_POINT('Ctrl Pts',(-33.5805004332759,2.93820509012,304.062738432489));
#18131=CARTESIAN_POINT('Ctrl Pts',(-33.488526091266,2.92980438598327,304.057758340228));
#18132=CARTESIAN_POINT('Ctrl Pts',(-33.3964673617753,2.92139597410716,304.052773678678));
#18133=CARTESIAN_POINT('Ctrl Pts',(-33.304842742193,2.9086477291594,304.047789017128));
#18134=CARTESIAN_POINT('Ctrl Pts',(-33.2140917891522,2.89163652674748,304.042804355577));
#18135=CARTESIAN_POINT('Ctrl Pts',(-33.1232994960559,2.87461757517117,304.037817423349));
#18136=CARTESIAN_POINT('Ctrl Pts',(-33.0333821047478,2.85333190480005,304.032830491121));
#18137=CARTESIAN_POINT('Ctrl Pts',(-32.9447663500711,2.82790697420564,304.027843558893));
#18138=CARTESIAN_POINT('Ctrl Pts',(-32.8560038399768,2.80243993770894,304.02284836787));
#18139=CARTESIAN_POINT('Ctrl Pts',(-32.7685477034634,2.77282009480686,304.017853176847));
#18140=CARTESIAN_POINT('Ctrl Pts',(-32.6828068523918,2.7392239423821,304.012857985824));
#18141=CARTESIAN_POINT('Ctrl Pts',(-32.6092424126289,2.71039891789928,304.008572182447));
#18142=CARTESIAN_POINT('Ctrl Pts',(-32.536940474007,2.67864765089728,304.004286379069));
#18143=CARTESIAN_POINT('Ctrl Pts',(-32.4661441993221,2.64410822562003,304.000000575692));
#18144=CARTESIAN_POINT('Ctrl Pts',(-32.4661441993221,2.64410822562003,304.));
#18145=CARTESIAN_POINT('Ctrl Pts',(-32.4496278394245,2.63585700138036,304.));
#18146=CARTESIAN_POINT('Ctrl Pts',(-32.4331114795268,2.6276057771407,304.));
#18147=CARTESIAN_POINT('Ctrl Pts',(-32.4165951196292,2.61935455290104,304.));
#18148=CARTESIAN_POINT('Origin',(-33.7561270252576,0.,302.151410108095));
#18149=CARTESIAN_POINT('',(-32.4049121771464,-1.94920919778867,314.));
#18150=CARTESIAN_POINT('Ctrl Pts',(-32.4049121771464,-1.94920919778867,
314.));
#18151=CARTESIAN_POINT('Ctrl Pts',(-32.546952397172,-2.04767315668297,313.987706520162));
#18152=CARTESIAN_POINT('Ctrl Pts',(-32.6993597984201,-2.1303378470281,313.974877189416));
#18153=CARTESIAN_POINT('Ctrl Pts',(-32.9571916953468,-2.23563193038453,
313.954758328853));
#18154=CARTESIAN_POINT('Ctrl Pts',(-33.0575139549198,-2.26898502116613,
313.947268440236));
#18155=CARTESIAN_POINT('Ctrl Pts',(-33.1919371907971,-2.30390855521111,
313.937699059563));
#18156=CARTESIAN_POINT('Ctrl Pts',(-33.2243097112393,-2.3115958427466,313.935428300996));
#18157=CARTESIAN_POINT('Ctrl Pts',(-33.2793153484165,-2.32344087527509,
313.931624624882));
#18158=CARTESIAN_POINT('Ctrl Pts',(-33.3018658348899,-2.32795483446128,
313.930080595254));
#18159=CARTESIAN_POINT('Ctrl Pts',(-33.347557267435,-2.33641170649212,313.926981619148));
#18160=CARTESIAN_POINT('Ctrl Pts',(-33.3706982218082,-2.34034049083399,
313.925427277736));
#18161=CARTESIAN_POINT('Ctrl Pts',(-33.42928515672,-2.34939457623398,313.921527820823));
#18162=CARTESIAN_POINT('Ctrl Pts',(-33.464796649993,-2.35406187527999,313.919197146517));
#18163=CARTESIAN_POINT('Ctrl Pts',(-33.6879281557284,-2.37826128555859,
313.904729739823));
#18164=CARTESIAN_POINT('Ctrl Pts',(-33.8772083579459,-2.37615718787244,
313.893306804096));
#18165=CARTESIAN_POINT('Ctrl Pts',(-34.167251331297,-2.3381544080642,313.875257458118));
#18166=CARTESIAN_POINT('Ctrl Pts',(-34.2692421070532,-2.31790791933874,
313.868785711074));
#18167=CARTESIAN_POINT('Ctrl Pts',(-34.3908902770311,-2.28533609520776,
313.860568378906));
#18168=CARTESIAN_POINT('Ctrl Pts',(-34.4121343053052,-2.27932880839701,
313.85911434623));
#18169=CARTESIAN_POINT('Ctrl Pts',(-34.4462839737763,-2.26915518751873,
313.856741554283));
#18170=CARTESIAN_POINT('Ctrl Pts',(-34.459243676734,-2.26517302436779,313.855832769321));
#18171=CARTESIAN_POINT('Ctrl Pts',(-34.4850303036276,-2.25700688965477,
313.854006537219));
#18172=CARTESIAN_POINT('Ctrl Pts',(-34.4978569923614,-2.25282416468677,
313.853089152264));
#18173=CARTESIAN_POINT('Ctrl Pts',(-34.5315680215517,-2.24151205800829,
313.850655593389));
#18174=CARTESIAN_POINT('Ctrl Pts',(-34.5523893071388,-2.23420037944764,
313.849129638672));
#18175=CARTESIAN_POINT('Ctrl Pts',(-34.6674173892997,-2.19199460440589,
313.840583150255));
#18176=CARTESIAN_POINT('Ctrl Pts',(-34.7594270324946,-2.15143567467892,
313.833314737358));
#18177=CARTESIAN_POINT('Ctrl Pts',(-34.9675437451218,-2.04343623286027,
313.816227684194));
#18178=CARTESIAN_POINT('Ctrl Pts',(-35.0810725147094,-1.97172185827824,
313.806408802031));
#18179=CARTESIAN_POINT('Ctrl Pts',(-35.2488180842235,-1.84469587552593,
313.791410683873));
#18180=CARTESIAN_POINT('Ctrl Pts',(-35.3074395161469,-1.79567848113724,
313.786057415392));
#18181=CARTESIAN_POINT('Ctrl Pts',(-35.3858820445179,-1.72337315872949,
313.778735173008));
#18182=CARTESIAN_POINT('Ctrl Pts',(-35.4077701362672,-1.70240760355948,
313.776673022591));
#18183=CARTESIAN_POINT('Ctrl Pts',(-35.4451893470748,-1.66516431478187,
313.773112134324));
#18184=CARTESIAN_POINT('Ctrl Pts',(-35.4609014395612,-1.64907488566002,
313.771605494546));
#18185=CARTESIAN_POINT('Ctrl Pts',(-35.493140037088,-1.6151087792166,313.768488564435));
#18186=CARTESIAN_POINT('Ctrl Pts',(-35.5096249735042,-1.59719616553267,
313.766880158734));
#18187=CARTESIAN_POINT('Ctrl Pts',(-35.5526638902841,-1.5489601850766,313.76263860479));
#18188=CARTESIAN_POINT('Ctrl Pts',(-35.5787263229804,-1.51820765015145,
313.760025781307));
#18189=CARTESIAN_POINT('Ctrl Pts',(-35.6993112958567,-1.36833927619302,
313.747687238571));
#18190=CARTESIAN_POINT('Ctrl Pts',(-35.7830192973965,-1.24097993977316,
313.738382399714));
#18191=CARTESIAN_POINT('Ctrl Pts',(-35.897886604779,-1.02319512526853,313.723283990641));
#18192=CARTESIAN_POINT('Ctrl Pts',(-35.9368094258337,-0.937381690122294,
313.717508739824));
#18193=CARTESIAN_POINT('Ctrl Pts',(-35.9889492360539,-0.80146648230257,
313.708313282547));
#18194=CARTESIAN_POINT('Ctrl Pts',(-36.0058029628861,-0.752861784914797,
313.705015106783));
#18195=CARTESIAN_POINT('Ctrl Pts',(-36.0265141381641,-0.686205521457368,
313.700430320496));
#18196=CARTESIAN_POINT('Ctrl Pts',(-36.0317617784603,-0.668597096852082,
313.699213415459));
#18197=CARTESIAN_POINT('Ctrl Pts',(-36.0403013893281,-0.638676691086577,
313.697133124901));
#18198=CARTESIAN_POINT('Ctrl Pts',(-36.0436997804577,-0.626395501086884,
313.696275672194));
#18199=CARTESIAN_POINT('Ctrl Pts',(-36.0507301357466,-0.600168548460251,
313.694435980716));
#18200=CARTESIAN_POINT('Ctrl Pts',(-36.0543341787238,-0.586216319855497,
313.693452326629));
#18201=CARTESIAN_POINT('Ctrl Pts',(-36.0643104034602,-0.546089080092318,
313.690610757855));
#18202=CARTESIAN_POINT('Ctrl Pts',(-36.0703638315002,-0.519838092049073,
313.688736599195));
#18203=CARTESIAN_POINT('Ctrl Pts',(-36.0974819260065,-0.392359244398201,
313.679580186892));
#18204=CARTESIAN_POINT('Ctrl Pts',(-36.1123572848319,-0.289937465168354,
313.672060948067));
#18205=CARTESIAN_POINT('Ctrl Pts',(-36.128133741848,-0.0903387662782653,
313.657439242264));
#18206=CARTESIAN_POINT('Ctrl Pts',(-36.1298446285413,0.00658624064446136,
313.650353717353));
#18207=CARTESIAN_POINT('Ctrl Pts',(-36.1214038017457,0.200112860721583,
313.636406114048));
#18208=CARTESIAN_POINT('Ctrl Pts',(-36.111259420544,0.296538515661029,313.629557095198));
#18209=CARTESIAN_POINT('Ctrl Pts',(-36.0899023192132,0.423951591307785,
313.62066387304));
#18210=CARTESIAN_POINT('Ctrl Pts',(-36.0839099567062,0.455707010347677,
313.618460013956));
#18211=CARTESIAN_POINT('Ctrl Pts',(-36.0726202738657,0.509479384929339,
313.614747757973));
#18212=CARTESIAN_POINT('Ctrl Pts',(-36.067653359524,0.531560234068789,313.613229033218));
#18213=CARTESIAN_POINT('Ctrl Pts',(-36.0575692570726,0.573572110180929,
313.610349055141));
#18214=CARTESIAN_POINT('Ctrl Pts',(-36.0525072964069,0.593514117459212,
313.608986169565));
#18215=CARTESIAN_POINT('Ctrl Pts',(-36.0385100200212,0.645795179190906,
313.605422488699));
#18216=CARTESIAN_POINT('Ctrl Pts',(-36.0291467352573,0.678015583222187,
313.603235738591));
#18217=CARTESIAN_POINT('Ctrl Pts',(-35.9881147377419,0.808791307870451,
313.594384793789));
#18218=CARTESIAN_POINT('Ctrl Pts',(-35.9506928190437,0.905426474581189,
313.587908386437));
#18219=CARTESIAN_POINT('Ctrl Pts',(-35.8560951271363,1.10904012995237,313.574055173609));
#18220=CARTESIAN_POINT('Ctrl Pts',(-35.7967986431042,1.21469920176365,313.566732922974));
#18221=CARTESIAN_POINT('Ctrl Pts',(-35.6842453467343,1.38357353035682,313.554153580709));
#18222=CARTESIAN_POINT('Ctrl Pts',(-35.6352886229486,1.44936702732116,313.548997777689));
#18223=CARTESIAN_POINT('Ctrl Pts',(-35.5696865950633,1.52860644025295,313.542277456499));
#18224=CARTESIAN_POINT('Ctrl Pts',(-35.5561296798544,1.54454728979497,313.540897791833));
#18225=CARTESIAN_POINT('Ctrl Pts',(-35.5337187495388,1.57020330700864,313.538627664557));
#18226=CARTESIAN_POINT('Ctrl Pts',(-35.5249913545983,1.58002839680919,313.537746141578));
#18227=CARTESIAN_POINT('Ctrl Pts',(-35.5071369081008,1.59979516842411,313.535946585833));
#18228=CARTESIAN_POINT('Ctrl Pts',(-35.4980058704805,1.60973235553793,313.535028322804));
#18229=CARTESIAN_POINT('Ctrl Pts',(-35.4734912843044,1.63595844722554,313.532569729515));
#18230=CARTESIAN_POINT('Ctrl Pts',(-35.4579612824317,1.65210777743187,313.5310191106));
#18231=CARTESIAN_POINT('Ctrl Pts',(-35.3579117961932,1.75323958875642,313.521086431675));
#18232=CARTESIAN_POINT('Ctrl Pts',(-35.2672886449006,1.83192478525135,313.51235148184));
#18233=CARTESIAN_POINT('Ctrl Pts',(-35.080206232925,1.97100101161773,313.495324689864));
#18234=CARTESIAN_POINT('Ctrl Pts',(-34.984561623233,2.0319898926767,313.487056435203));
#18235=CARTESIAN_POINT('Ctrl Pts',(-34.8170163848832,2.12265698300166,313.473467876795));
#18236=CARTESIAN_POINT('Ctrl Pts',(-34.747355239735,2.1560676693847,313.468052939947));
#18237=CARTESIAN_POINT('Ctrl Pts',(-34.6482245646911,2.19778981212911,313.460670121061));
#18238=CARTESIAN_POINT('Ctrl Pts',(-34.6200438056141,2.2090192447726,313.458606034392));
#18239=CARTESIAN_POINT('Ctrl Pts',(-34.5706848275723,2.22759863218599,313.455048800781));
#18240=CARTESIAN_POINT('Ctrl Pts',(-34.5496040529138,2.23519447602278,313.453547603489));
#18241=CARTESIAN_POINT('Ctrl Pts',(-34.505581055095,2.25035555175753,313.450448632843));
#18242=CARTESIAN_POINT('Ctrl Pts',(-34.4826244620117,2.25787134242534,313.448852641262));
#18243=CARTESIAN_POINT('Ctrl Pts',(-34.4216084089499,2.27682048568616,313.444660505233));
#18244=CARTESIAN_POINT('Ctrl Pts',(-34.3833686727503,2.28765058682674,313.442084061991));
#18245=CARTESIAN_POINT('Ctrl Pts',(-34.1889463169214,2.33747196546371,313.429207272684));
#18246=CARTESIAN_POINT('Ctrl Pts',(-34.0293544471349,2.3614530994093,313.419391192156));
#18247=CARTESIAN_POINT('Ctrl Pts',(-33.7806442261837,2.37325557290962,313.404119197688));
#18248=CARTESIAN_POINT('Ctrl Pts',(-33.6925785497909,2.37253087335058,313.398707720936));
#18249=CARTESIAN_POINT('Ctrl Pts',(-33.5554374422751,2.3637607162759,313.39001598739));
#18250=CARTESIAN_POINT('Ctrl Pts',(-33.5062262736265,2.35906546636591,313.386842940111));
#18251=CARTESIAN_POINT('Ctrl Pts',(-33.4392539520886,2.35055670877303,313.382406970114));
#18252=CARTESIAN_POINT('Ctrl Pts',(-33.4213335149318,2.34807125976028,313.38120839125));
#18253=CARTESIAN_POINT('Ctrl Pts',(-33.3908933985363,2.34349387427042,313.379149980199));
#18254=CARTESIAN_POINT('Ctrl Pts',(-33.3783590314818,2.34150602736475,313.378295826024));
#18255=CARTESIAN_POINT('Ctrl Pts',(-33.3514543302274,2.33701750095182,313.376447456013));
#18256=CARTESIAN_POINT('Ctrl Pts',(-33.3370909008514,2.3344848442745,313.375451661093));
#18257=CARTESIAN_POINT('Ctrl Pts',(-33.2963533547509,2.32691366546731,313.372603467335));
#18258=CARTESIAN_POINT('Ctrl Pts',(-33.2700410606749,2.32155967373467,313.370735247782));
#18259=CARTESIAN_POINT('Ctrl Pts',(-33.1398084133472,2.29274917163599,313.361364416972));
#18260=CARTESIAN_POINT('Ctrl Pts',(-33.0374675207498,2.26275760058699,313.353611370755));
#18261=CARTESIAN_POINT('Ctrl Pts',(-32.846386320345,2.19248583290265,313.338745192836));
#18262=CARTESIAN_POINT('Ctrl Pts',(-32.7574124410887,2.15341433065302,313.331649495554));
#18263=CARTESIAN_POINT('Ctrl Pts',(-32.6707032669284,2.10880380957248,313.324639106241));
#18264=CARTESIAN_POINT('Ctrl Pts',(-32.6703261471224,2.1086096593382,313.324608614338));
#18265=CARTESIAN_POINT('Ctrl Pts',(-32.6699490794749,2.10841540797709,313.324578124683));
#18266=CARTESIAN_POINT('',(-35.1331518153888,-1.93106208855754,314.));
#18267=CARTESIAN_POINT('Origin',(-33.7561270252576,0.,314.));
#18268=CARTESIAN_POINT('',(-36.1278767566871,0.00112870026910663,313.848589891954));
#18269=CARTESIAN_POINT('Ctrl Pts',(-36.1278767566871,0.00112870026910672,
313.848589891954));
#18270=CARTESIAN_POINT('Ctrl Pts',(-36.1279148957173,-0.0790132446041546,
313.854008225009));
#18271=CARTESIAN_POINT('Ctrl Pts',(-36.123886772926,-0.159300080416319,
313.859426558064));
#18272=CARTESIAN_POINT('Ctrl Pts',(-36.1157746507306,-0.239293013060521,
313.864844891119));
#18273=CARTESIAN_POINT('Ctrl Pts',(-36.1073434386814,-0.322432463048055,
313.870476353989));
#18274=CARTESIAN_POINT('Ctrl Pts',(-36.094500195761,-0.405253930370168,
313.876107816859));
#18275=CARTESIAN_POINT('Ctrl Pts',(-36.0772847864738,-0.487262465254211,
313.881739279729));
#18276=CARTESIAN_POINT('Ctrl Pts',(-36.0607750699741,-0.565909312326557,
313.887139898089));
#18277=CARTESIAN_POINT('Ctrl Pts',(-36.0402446877037,-0.643808064903195,
313.892540516448));
#18278=CARTESIAN_POINT('Ctrl Pts',(-36.0157815835671,-0.720527126214705,
313.897941134808));
#18279=CARTESIAN_POINT('Ctrl Pts',(-35.9913404357878,-0.79717732990626,
313.903336905953));
#18280=CARTESIAN_POINT('Ctrl Pts',(-35.9629737164686,-0.872649518442759,
313.908732677098));
#18281=CARTESIAN_POINT('Ctrl Pts',(-35.9308198228037,-0.946524853768198,
313.914128448244));
#18282=CARTESIAN_POINT('Ctrl Pts',(-35.8986858374103,-1.02035444874764,
313.919520878566));
#18283=CARTESIAN_POINT('Ctrl Pts',(-35.8627695184512,-1.0925887433214,313.924913308888));
#18284=CARTESIAN_POINT('Ctrl Pts',(-35.8232578094233,-1.16282775321819,
313.93030573921));
#18285=CARTESIAN_POINT('Ctrl Pts',(-35.7837595696115,-1.23304281921512,
313.935696331297));
#18286=CARTESIAN_POINT('Ctrl Pts',(-35.7406685988365,-1.30126356100973,
313.941086923384));
#18287=CARTESIAN_POINT('Ctrl Pts',(-35.6942177298364,-1.36711465624701,
313.946477515471));
#18288=CARTESIAN_POINT('Ctrl Pts',(-35.647754830922,-1.43298280569759,313.951869503621));
#18289=CARTESIAN_POINT('Ctrl Pts',(-35.5979305514185,-1.49647971103082,
313.957261491771));
#18290=CARTESIAN_POINT('Ctrl Pts',(-35.5450205211567,-1.55725981224386,
313.962653479922));
#18291=CARTESIAN_POINT('Ctrl Pts',(-35.4921025627892,-1.61804902082397,
313.968046276014));
#18292=CARTESIAN_POINT('Ctrl Pts',(-35.436098236994,-1.6761202813854,313.973439072107));
#18293=CARTESIAN_POINT('Ctrl Pts',(-35.3773216657082,-1.73116319284876,
313.9788318682));
#18294=CARTESIAN_POINT('Ctrl Pts',(-35.3184964663978,-1.78625164334224,
313.984229125952));
#18295=CARTESIAN_POINT('Ctrl Pts',(-35.2568947803512,-1.83830644365573,
313.989626383703));
#18296=CARTESIAN_POINT('Ctrl Pts',(-35.1928650153576,-1.88705644067775,
313.995023641455));
#18297=CARTESIAN_POINT('Ctrl Pts',(-35.1731861906162,-1.90203920139284,
313.996682427637));
#18298=CARTESIAN_POINT('Ctrl Pts',(-35.1532782346255,-1.91671010143613,
313.998341213818));
#18299=CARTESIAN_POINT('Ctrl Pts',(-35.1331518153888,-1.93106208855753,
314.));
#18300=CARTESIAN_POINT('Ctrl Pts',(-32.6699490794746,2.10841540797695,313.522886073942));
#18301=CARTESIAN_POINT('Ctrl Pts',(-32.6716174179545,2.10927487450148,313.523012757125));
#18302=CARTESIAN_POINT('Ctrl Pts',(-32.6732867045892,2.11013232378011,313.523139440309));
#18303=CARTESIAN_POINT('Ctrl Pts',(-32.6749569340628,2.11098775373186,313.523266123492));
#18304=CARTESIAN_POINT('Ctrl Pts',(-32.7452259553958,2.14697695550172,313.52859587216));
#18305=CARTESIAN_POINT('Ctrl Pts',(-32.8174259095208,2.17952132864185,313.533925620827));
#18306=CARTESIAN_POINT('Ctrl Pts',(-32.8911850198945,2.20840969701243,313.539255369495));
#18307=CARTESIAN_POINT('Ctrl Pts',(-32.9648389334936,2.23725686419224,313.544577516764));
#18308=CARTESIAN_POINT('Ctrl Pts',(-33.0400471541795,2.26245821167335,313.549899664034));
#18309=CARTESIAN_POINT('Ctrl Pts',(-33.1164141623099,2.28384883814127,313.555221811303));
#18310=CARTESIAN_POINT('Ctrl Pts',(-33.1926946841532,2.30521523954253,313.560537931195));
#18311=CARTESIAN_POINT('Ctrl Pts',(-33.270130936211,2.32277936968305,313.565854051088));
#18312=CARTESIAN_POINT('Ctrl Pts',(-33.3483097391138,2.33642528740432,313.57117017098));
#18313=CARTESIAN_POINT('Ctrl Pts',(-33.4264402244559,2.35006277141422,313.576483005302));
#18314=CARTESIAN_POINT('Ctrl Pts',(-33.5053118887913,2.35978676889661,313.581795839624));
#18315=CARTESIAN_POINT('Ctrl Pts',(-33.5844999923704,2.36553212281769,313.587108673946));
#18316=CARTESIAN_POINT('Ctrl Pts',(-33.663663866723,2.37127571882973,313.592419882697));
#18317=CARTESIAN_POINT('Ctrl Pts',(-33.7431435204535,2.37304305460202,313.597731091449));
#18318=CARTESIAN_POINT('Ctrl Pts',(-33.8225091910446,2.37082084320293,313.6030423002));
#18319=CARTESIAN_POINT('Ctrl Pts',(-33.9018753451706,2.36859861826502,313.60835354131));
#18320=CARTESIAN_POINT('Ctrl Pts',(-33.981127045836,2.36238681243055,313.61366478242));
#18321=CARTESIAN_POINT('Ctrl Pts',(-34.059836132218,2.35222423268899,313.61897602353));
#18322=CARTESIAN_POINT('Ctrl Pts',(-34.1386265621813,2.34205115021299,313.624292753655));
#18323=CARTESIAN_POINT('Ctrl Pts',(-34.2168727912834,2.32791919817414,313.62960948378));
#18324=CARTESIAN_POINT('Ctrl Pts',(-34.2941539597541,2.30991884711482,313.634926213905));
#18325=CARTESIAN_POINT('Ctrl Pts',(-34.3714735949446,2.29190953637654,313.640245590433));
#18326=CARTESIAN_POINT('Ctrl Pts',(-34.4478267611363,2.27002812078966,313.645564966962));
#18327=CARTESIAN_POINT('Ctrl Pts',(-34.5228074577539,2.24441510797964,313.650884343491));
#18328=CARTESIAN_POINT('Ctrl Pts',(-34.5979275613812,2.21875447446609,313.65621361001));
#18329=CARTESIAN_POINT('Ctrl Pts',(-34.6716696596955,2.18934855474684,313.661542876529));
#18330=CARTESIAN_POINT('Ctrl Pts',(-34.7436476134916,2.15638613200745,313.666872143048));
#18331=CARTESIAN_POINT('Ctrl Pts',(-34.8125527934063,2.12483089113858,313.671973900586));
#18332=CARTESIAN_POINT('Ctrl Pts',(-34.8798410874767,2.09001683724949,313.677075658123));
#18333=CARTESIAN_POINT('Ctrl Pts',(-34.9451978764374,2.05214730791302,313.682177415661));
#18334=CARTESIAN_POINT('Ctrl Pts',(-35.013046995834,2.01283365345862,313.687473724764));
#18335=CARTESIAN_POINT('Ctrl Pts',(-35.0790828745383,1.97007105799335,313.692770033867));
#18336=CARTESIAN_POINT('Ctrl Pts',(-35.1429293220549,1.92405235170398,313.698066342969));
#18337=CARTESIAN_POINT('Ctrl Pts',(-35.2066825731113,1.87810081877663,313.703354921066));
#18338=CARTESIAN_POINT('Ctrl Pts',(-35.2682523544018,1.82890288543903,313.708643499163));
#18339=CARTESIAN_POINT('Ctrl Pts',(-35.3272881060166,1.77669663161954,313.71393207726));
#18340=CARTESIAN_POINT('Ctrl Pts',(-35.386431186956,1.72439546477183,313.719230270201));
#18341=CARTESIAN_POINT('Ctrl Pts',(-35.4430306056107,1.66907528072418,313.724528463141));
#18342=CARTESIAN_POINT('Ctrl Pts',(-35.4967642823664,1.6110183120203,313.729826656081));
#18343=CARTESIAN_POINT('Ctrl Pts',(-35.5503054039893,1.55316939100624,313.735105862898));
#18344=CARTESIAN_POINT('Ctrl Pts',(-35.6010009517321,1.49260360694134,313.740385069715));
#18345=CARTESIAN_POINT('Ctrl Pts',(-35.6485679839444,1.42963816414665,313.745664276531));
#18346=CARTESIAN_POINT('Ctrl Pts',(-35.6961206913763,1.36669168335346,313.750941893518));
#18347=CARTESIAN_POINT('Ctrl Pts',(-35.7405464664373,1.30134735762143,313.756219510505));
#18348=CARTESIAN_POINT('Ctrl Pts',(-35.7816031421524,1.23395484617098,313.761497127492));
#18349=CARTESIAN_POINT('Ctrl Pts',(-35.8226606883943,1.1665609057935,313.76677485638));
#18350=CARTESIAN_POINT('Ctrl Pts',(-35.8603487469998,1.09711910072152,313.772052585269));
#18351=CARTESIAN_POINT('Ctrl Pts',(-35.8944697687086,1.02600603021152,313.777330314157));
#18352=CARTESIAN_POINT('Ctrl Pts',(-35.9288201111352,0.954415022653908,
313.78264351363));
#18353=CARTESIAN_POINT('Ctrl Pts',(-35.9595550682039,0.881130636100437,
313.787956713103));
#18354=CARTESIAN_POINT('Ctrl Pts',(-35.9865220636178,0.806558141337787,
313.793269912575));
#18355=CARTESIAN_POINT('Ctrl Pts',(-36.013352938898,0.732362062924119,313.798556292842));
#18356=CARTESIAN_POINT('Ctrl Pts',(-36.0364537219332,0.656891326621502,
313.803842673108));
#18357=CARTESIAN_POINT('Ctrl Pts',(-36.0557246703262,0.580558983476379,
313.809129053374));
#18358=CARTESIAN_POINT('Ctrl Pts',(-36.0751422686538,0.503645759052962,
313.81445566245));
#18359=CARTESIAN_POINT('Ctrl Pts',(-36.0906714086751,0.425858242206631,
313.819782271526));
#18360=CARTESIAN_POINT('Ctrl Pts',(-36.1022630534639,0.347625947898785,
313.825108880602));
#18361=CARTESIAN_POINT('Ctrl Pts',(-36.1138546982526,0.269393653590927,
313.830435489678));
#18362=CARTESIAN_POINT('Ctrl Pts',(-36.1215088749716,0.19071707224102,313.835762098754));
#18363=CARTESIAN_POINT('Ctrl Pts',(-36.1252298902417,0.112025343668419,
313.84108870783));
#18364=CARTESIAN_POINT('Ctrl Pts',(-36.1269765937627,0.0750861995389757,
313.843589102522));
#18365=CARTESIAN_POINT('Ctrl Pts',(-36.1278591566815,0.038111753064283,
313.846089497213));
#18366=CARTESIAN_POINT('Ctrl Pts',(-36.1278767566867,0.00112870099215847,
313.848589891905));
#18367=CARTESIAN_POINT('Ctrl Pts',(-34.7933121966354,2.12810918362782,303.66825685423));
#18368=CARTESIAN_POINT('Ctrl Pts',(-35.5015959476307,1.78291007010875,303.721227284953));
#18369=CARTESIAN_POINT('Ctrl Pts',(-36.5334100271131,0.333763633321939,
303.827168146399));
#18370=CARTESIAN_POINT('Ctrl Pts',(-35.5413299366473,-2.15794291786034,
303.986079438568));
#18371=CARTESIAN_POINT('Ctrl Pts',(-32.9089357156284,-2.66755271063891,
304.144990730738));
#18372=CARTESIAN_POINT('Ctrl Pts',(-31.0548666733256,-0.733421038154457,
304.303902022907));
#18373=CARTESIAN_POINT('Ctrl Pts',(-31.6765983504046,1.8740003336691,304.462813315076));
#18374=CARTESIAN_POINT('Ctrl Pts',(-34.2052449936392,2.76288312959717,304.621724607246));
#18375=CARTESIAN_POINT('Ctrl Pts',(-36.3219606220703,1.11889486817046,304.780635899415));
#18376=CARTESIAN_POINT('Ctrl Pts',(-36.0863485172746,-1.55101144960505,
304.939547191584));
#18377=CARTESIAN_POINT('Ctrl Pts',(-33.7143042574469,-2.79887542003478,
305.098458483753));
#18378=CARTESIAN_POINT('Ctrl Pts',(-31.3806218553374,-1.48069437689556,
305.257369775923));
#18379=CARTESIAN_POINT('Ctrl Pts',(-31.224842213905,1.19502694802466,305.416281068092));
#18380=CARTESIAN_POINT('Ctrl Pts',(-33.3897996861207,2.775118803617,305.575192360261));
#18381=CARTESIAN_POINT('Ctrl Pts',(-35.8906115960418,1.81092775317516,305.734103652431));
#18382=CARTESIAN_POINT('Ctrl Pts',(-36.4344857504044,-0.813559522228039,
305.8930149446));
#18383=CARTESIAN_POINT('Ctrl Pts',(-34.5227860158784,-2.69215848558538,
306.051926236769));
#18384=CARTESIAN_POINT('Ctrl Pts',(-31.908198004047,-2.102532305537,306.210837528939));
#18385=CARTESIAN_POINT('Ctrl Pts',(-30.9878286152358,0.41473814013526,306.369748821108));
#18386=CARTESIAN_POINT('Ctrl Pts',(-32.6054912639837,2.55176821696523,306.528660113277));
#18387=CARTESIAN_POINT('Ctrl Pts',(-35.2780800389393,2.34928558602826,306.687571405446));
#18388=CARTESIAN_POINT('Ctrl Pts',(-36.5553115068302,-0.00706961484117916,
306.846482697616));
#18389=CARTESIAN_POINT('Ctrl Pts',(-35.2661940011202,-2.35694324448151,
307.005393989785));
#18390=CARTESIAN_POINT('Ctrl Pts',(-32.5926165407175,-2.54592362172222,
307.164305281954));
#18391=CARTESIAN_POINT('Ctrl Pts',(-30.9857690329855,-0.400749709361767,
307.323216574124));
#18392=CARTESIAN_POINT('Ctrl Pts',(-31.9188417860902,2.11183964440955,307.482127866293));
#18393=CARTESIAN_POINT('Ctrl Pts',(-34.5363748202831,2.68825168330378,307.641039158462));
#18394=CARTESIAN_POINT('Ctrl Pts',(-36.4385608892421,0.800020187051445,
307.799950450632));
#18395=CARTESIAN_POINT('Ctrl Pts',(-35.8814373175924,-1.82168600355083,
307.958861742801));
#18396=CARTESIAN_POINT('Ctrl Pts',(-33.3757862682556,-2.77323360769926,
308.11777303497));
#18397=CARTESIAN_POINT('Ctrl Pts',(-31.2188393204144,-1.18222452907508,
308.27668432714));
#18398=CARTESIAN_POINT('Ctrl Pts',(-31.3881290776734,1.49267191791212,308.435595619309));
#18399=CARTESIAN_POINT('Ctrl Pts',(-33.7284472653066,2.79905654912215,308.594506911478));
#18400=CARTESIAN_POINT('Ctrl Pts',(-36.0941428169125,1.53920950239539,308.753418203648));
#18401=CARTESIAN_POINT('Ctrl Pts',(-36.3162981853304,-1.13181595916618,
308.912329495817));
#18402=CARTESIAN_POINT('Ctrl Pts',(-34.1912368338946,-2.76516964917568,
309.071240787986));
#18403=CARTESIAN_POINT('Ctrl Pts',(-31.6672580062641,-1.86335985675752,
309.230152080156));
#18404=CARTESIAN_POINT('Ctrl Pts',(-31.0583965596219,0.746815953951488,
309.389063372325));
#18405=CARTESIAN_POINT('Ctrl Pts',(-32.9228689874342,2.67229578765376,309.547974664494));
#18406=CARTESIAN_POINT('Ctrl Pts',(-35.5512892437397,2.14776077428841,309.706885956663));
#18407=CARTESIAN_POINT('Ctrl Pts',(-36.5338684563932,-0.345884772855582,
309.865797248833));
#18408=CARTESIAN_POINT('Ctrl Pts',(-34.969758122513,-2.52241616197692,310.024708541002));
#18409=CARTESIAN_POINT('Ctrl Pts',(-32.2929662431881,-2.38634537726121,
310.183619833172));
#18410=CARTESIAN_POINT('Ctrl Pts',(-30.9576297730183,-0.0624248677114656,
310.342531125341));
#18411=CARTESIAN_POINT('Ctrl Pts',(-32.1880122064702,2.31872802423598,310.50144241751));
#18412=CARTESIAN_POINT('Ctrl Pts',(-34.8560740328554,2.5740241470846,310.66035370968));
#18413=CARTESIAN_POINT('Ctrl Pts',(-36.5156821890243,0.469402854123652,
310.819265001849));
#18414=CARTESIAN_POINT('Ctrl Pts',(-35.6452743329216,-2.06557647898139,
310.978176294018));
#18415=CARTESIAN_POINT('Ctrl Pts',(-33.0428580095468,-2.70679349036151,
311.137087586187));
#18416=CARTESIAN_POINT('Ctrl Pts',(-31.0943811349663,-0.86636748976959,
311.295998878356));
#18417=CARTESIAN_POINT('Ctrl Pts',(-31.5862467830163,1.76836181184454,311.454910170526));
#18418=CARTESIAN_POINT('Ctrl Pts',(-34.0675024665792,2.78182110387257,311.613821462695));
#18419=CARTESIAN_POINT('Ctrl Pts',(-36.2632830024395,1.24485077935404,311.772732754865));
#18420=CARTESIAN_POINT('Ctrl Pts',(-36.1604518779547,-1.43342447057343,
311.931644047034));
#18421=CARTESIAN_POINT('Ctrl Pts',(-33.8532877870383,-2.79750601070989,
312.090555339203));
#18422=CARTESIAN_POINT('Ctrl Pts',(-31.4570432481482,-1.5967798810487,312.249466631373));
#18423=CARTESIAN_POINT('Ctrl Pts',(-31.1686484045087,1.06791153063105,312.408377923542));
#18424=CARTESIAN_POINT('Ctrl Pts',(-33.2524995915862,2.75350906460025,312.567289215711));
#18425=CARTESIAN_POINT('Ctrl Pts',(-35.7981008484644,1.91465705127629,312.72620050788));
#18426=CARTESIAN_POINT('Ctrl Pts',(-36.4715489807011,-0.679640623010668,
312.88511180005));
#18427=CARTESIAN_POINT('Ctrl Pts',(-34.6555073427497,-2.65072540672241,
313.044023092219));
#18428=CARTESIAN_POINT('Ctrl Pts',(-32.0147597975284,-2.19179308747854,
313.202934384388));
#18429=CARTESIAN_POINT('Ctrl Pts',(-30.970820086982,0.277090540655818,313.361845676558));
#18430=CARTESIAN_POINT('Ctrl Pts',(-32.4798917398762,2.49094240710133,313.520756968727));
#18431=CARTESIAN_POINT('Ctrl Pts',(-35.1603047572903,2.42321108623274,313.679668260896));
#18432=CARTESIAN_POINT('Ctrl Pts',(-36.5506207995528,0.129250313862038,
313.838606176025));
#18433=CARTESIAN_POINT('Ctrl Pts',(-35.7717615680654,-1.47086186108563,
313.94457366043));
#18434=CARTESIAN_POINT('Ctrl Pts',(-35.1296610793728,-1.92821312738253,
313.997570714112));
#18435=CARTESIAN_POINT('Ctrl Pts',(-34.8778062619321,2.30147513725125,303.779604659097));
#18436=CARTESIAN_POINT('Ctrl Pts',(-35.6437901952638,1.92815445273122,303.83257508982));
#18437=CARTESIAN_POINT('Ctrl Pts',(-36.7596607852054,0.360953615405971,
303.938515951266));
#18438=CARTESIAN_POINT('Ctrl Pts',(-35.686761105088,-2.33373927018,304.097427243436));
#18439=CARTESIAN_POINT('Ctrl Pts',(-32.8399194591199,-2.8848643143285,304.256338535605));
#18440=CARTESIAN_POINT('Ctrl Pts',(-30.8348090839403,-0.793169024143786,
304.415249827774));
#18441=CARTESIAN_POINT('Ctrl Pts',(-31.5071899974042,2.02666536487924,304.574161119944));
#18442=CARTESIAN_POINT('Ctrl Pts',(-34.2418322916392,2.98796080521536,304.733072412113));
#18443=CARTESIAN_POINT('Ctrl Pts',(-36.5309857001877,1.2100453962153,304.891983704282));
#18444=CARTESIAN_POINT('Ctrl Pts',(-36.2761795063165,-1.67736426134529,
305.050894996451));
#18445=CARTESIAN_POINT('Ctrl Pts',(-33.7108971747275,-3.02688519979633,
305.209806288621));
#18446=CARTESIAN_POINT('Ctrl Pts',(-31.1871018412851,-1.60131882354062,
305.36871758079));
#18447=CARTESIAN_POINT('Ctrl Pts',(-31.0186316451104,1.292379559462,305.52762887296));
#18448=CARTESIAN_POINT('Ctrl Pts',(-33.3599569087968,3.00119325576856,305.686540165129));
#18449=CARTESIAN_POINT('Ctrl Pts',(-36.0644969191988,1.95845459027906,305.845451457298));
#18450=CARTESIAN_POINT('Ctrl Pts',(-36.6526776637248,-0.879835972461675,
306.004362749467));
#18451=CARTESIAN_POINT('Ctrl Pts',(-34.5852417244649,-2.91147459340051,
306.163274041637));
#18452=CARTESIAN_POINT('Ctrl Pts',(-31.7576568666583,-2.27381464432759,
306.322185333806));
#18453=CARTESIAN_POINT('Ctrl Pts',(-30.7623097849709,0.448524692874981,
306.481096625975));
#18454=CARTESIAN_POINT('Ctrl Pts',(-32.5117549709583,2.75964746196053,306.640007918145));
#18455=CARTESIAN_POINT('Ctrl Pts',(-35.4020656114921,2.54066962735892,306.798919210314));
#18456=CARTESIAN_POINT('Ctrl Pts',(-36.7833464642229,-0.00764553948268389,
306.957830502483));
#18457=CARTESIAN_POINT('Ctrl Pts',(-35.389211280177,-2.54895111529913,307.116741794653));
#18458=CARTESIAN_POINT('Ctrl Pts',(-32.4978314111505,-2.7533267380322,307.275653086822));
#18459=CARTESIAN_POINT('Ctrl Pts',(-30.7600824192988,-0.433396697618922,
307.434564378991));
#18460=CARTESIAN_POINT('Ctrl Pts',(-31.7691677420999,2.28388020354508,307.593475671161));
#18461=CARTESIAN_POINT('Ctrl Pts',(-34.5999375378766,2.90724952431741,307.75238696333));
#18462=CARTESIAN_POINT('Ctrl Pts',(-36.6570847828653,0.865193658278026,
307.911298255499));
#18463=CARTESIAN_POINT('Ctrl Pts',(-36.054575260143,-1.97008925919095,308.070209547668));
#18464=CARTESIAN_POINT('Ctrl Pts',(-33.3448018908812,-2.99915448277377,
308.229120839838));
#18465=CARTESIAN_POINT('Ctrl Pts',(-31.0121397272021,-1.27853419422617,
308.388032132007));
#18466=CARTESIAN_POINT('Ctrl Pts',(-31.1952206378624,1.61427211234131,308.546943424176));
#18467=CARTESIAN_POINT('Ctrl Pts',(-33.7261923396586,3.02708108452555,308.705854716346));
#18468=CARTESIAN_POINT('Ctrl Pts',(-36.284608766886,1.66460087106293,308.864766008515));
#18469=CARTESIAN_POINT('Ctrl Pts',(-36.5248619742656,-1.22401910108982,
309.023677300684));
#18470=CARTESIAN_POINT('Ctrl Pts',(-34.2266829601957,-2.990433595616,309.182588592854));
#18471=CARTESIAN_POINT('Ctrl Pts',(-31.4970887441518,-2.01515806382118,
309.341499885023));
#18472=CARTESIAN_POINT('Ctrl Pts',(-30.8386265316591,0.807655153854402,
309.500411177192));
#18473=CARTESIAN_POINT('Ctrl Pts',(-32.8549878018948,2.88999378508484,309.659322469362));
#18474=CARTESIAN_POINT('Ctrl Pts',(-35.6975317449751,2.3227276404878,309.818233761531));
#18475=CARTESIAN_POINT('Ctrl Pts',(-36.7601565603275,-0.374062200945844,
309.9771450537));
#18476=CARTESIAN_POINT('Ctrl Pts',(-35.0686263169372,-2.72790424817124,
310.13605634587));
#18477=CARTESIAN_POINT('Ctrl Pts',(-32.1737701670472,-2.58074848645625,
310.294967638039));
#18478=CARTESIAN_POINT('Ctrl Pts',(-30.7296508006143,-0.067510296036245,
310.453878930208));
#18479=CARTESIAN_POINT('Ctrl Pts',(-32.0602660724647,2.50762270041502,310.612790222377));
#18480=CARTESIAN_POINT('Ctrl Pts',(-34.9456809775434,2.78371646660568,310.771701514547));
#18481=CARTESIAN_POINT('Ctrl Pts',(-36.740488752627,0.507642655946229,310.930612806716));
#18482=CARTESIAN_POINT('Ctrl Pts',(-35.7991733090868,-2.2338482193675,311.089524098886));
#18483=CARTESIAN_POINT('Ctrl Pts',(-32.9847517037003,-2.9273018356703,311.248435391055));
#18484=CARTESIAN_POINT('Ctrl Pts',(-30.8775425826384,-0.936945929639025,
311.407346683224));
#18485=CARTESIAN_POINT('Ctrl Pts',(-31.409477959152,1.91242102375915,311.566257975393));
#18486=CARTESIAN_POINT('Ctrl Pts',(-34.0928685994519,3.0084415574625,311.725169267563));
#18487=CARTESIAN_POINT('Ctrl Pts',(-36.4675279209855,1.34626227841713,311.884080559732));
#18488=CARTESIAN_POINT('Ctrl Pts',(-36.3563196812212,-1.5501980845402,312.042991851901));
#18489=CARTESIAN_POINT('Ctrl Pts',(-33.8612029674485,-3.02540423183745,
312.201903144071));
#18490=CARTESIAN_POINT('Ctrl Pts',(-31.2697488863056,-1.72686120814153,
312.36081443624));
#18491=CARTESIAN_POINT('Ctrl Pts',(-30.9578600192052,1.15490871212794,312.519725728409));
#18492=CARTESIAN_POINT('Ctrl Pts',(-33.2114716918049,2.97782308404421,312.678637020578));
#18493=CARTESIAN_POINT('Ctrl Pts',(-35.964449803611,2.07063417317869,312.837548312748));
#18494=CARTESIAN_POINT('Ctrl Pts',(-36.6927602420485,-0.735007399130949,
312.996459604917));
#18495=CARTESIAN_POINT('Ctrl Pts',(-34.7287751654779,-2.86666617774379,
313.155370897087));
#18496=CARTESIAN_POINT('Ctrl Pts',(-31.8728996935609,-2.37034703653308,
313.314282189256));
#18497=CARTESIAN_POINT('Ctrl Pts',(-30.7439156606475,0.299663661523098,
313.473193481425));
#18498=CARTESIAN_POINT('Ctrl Pts',(-32.3759235088286,2.69386649067301,313.632104773595));
#18499=CARTESIAN_POINT('Ctrl Pts',(-35.2746957920377,2.62061745242278,313.791016065764));
#18500=CARTESIAN_POINT('Ctrl Pts',(-36.7782736294934,0.13977966268081,313.949953980892));
#18501=CARTESIAN_POINT('Ctrl Pts',(-35.9359647994402,-1.59068530396026,
314.055921465297));
#18502=CARTESIAN_POINT('Ctrl Pts',(-35.2415557335371,-2.08529459208821,
314.108918518978));
#18503=CARTESIAN_POINT('Ctrl Pts',(-34.9623003272288,2.47484109087468,303.890952463964));
#18504=CARTESIAN_POINT('Ctrl Pts',(-35.785984442897,2.0733988353537,303.943922894687));
#18505=CARTESIAN_POINT('Ctrl Pts',(-36.9859115432976,0.388143597490006,
304.049863756133));
#18506=CARTESIAN_POINT('Ctrl Pts',(-35.8321922735287,-2.50953562249967,
304.208775048302));
#18507=CARTESIAN_POINT('Ctrl Pts',(-32.7709032026114,-3.10217591801808,
304.367686340471));
#18508=CARTESIAN_POINT('Ctrl Pts',(-30.614751494555,-0.852917010133116,
304.526597632641));
#18509=CARTESIAN_POINT('Ctrl Pts',(-31.337781644404,2.17933039608939,304.68550892481));
#18510=CARTESIAN_POINT('Ctrl Pts',(-34.2784195896392,3.21303848083357,304.844420216979));
#18511=CARTESIAN_POINT('Ctrl Pts',(-36.7400107783054,1.30119592426015,305.003331509149));
#18512=CARTESIAN_POINT('Ctrl Pts',(-36.4660104953585,-1.80371707308553,
305.162242801318));
#18513=CARTESIAN_POINT('Ctrl Pts',(-33.7074900920081,-3.25489497955788,
305.321154093487));
#18514=CARTESIAN_POINT('Ctrl Pts',(-30.9935818272327,-1.72194327018567,
305.480065385657));
#18515=CARTESIAN_POINT('Ctrl Pts',(-30.8124210763159,1.38973217089934,305.638976677826));
#18516=CARTESIAN_POINT('Ctrl Pts',(-33.330114131473,3.22726770792011,305.797887969995));
#18517=CARTESIAN_POINT('Ctrl Pts',(-36.2383822423557,2.10598142738296,305.956799262165));
#18518=CARTESIAN_POINT('Ctrl Pts',(-36.8708695770453,-0.94611242269531,
306.115710554334));
#18519=CARTESIAN_POINT('Ctrl Pts',(-34.6476974330514,-3.13079070121565,
306.274621846503));
#18520=CARTESIAN_POINT('Ctrl Pts',(-31.6071157292697,-2.44509698311818,
306.433533138673));
#18521=CARTESIAN_POINT('Ctrl Pts',(-30.5367909547061,0.482311245614701,
306.592444430842));
#18522=CARTESIAN_POINT('Ctrl Pts',(-32.418018677933,2.96752670695583,306.751355723011));
#18523=CARTESIAN_POINT('Ctrl Pts',(-35.5260511840449,2.73205366868956,306.91026701518));
#18524=CARTESIAN_POINT('Ctrl Pts',(-37.0113814216157,-0.00822146412418619,
307.06917830735));
#18525=CARTESIAN_POINT('Ctrl Pts',(-35.5122285592338,-2.74095898611676,
307.228089599519));
#18526=CARTESIAN_POINT('Ctrl Pts',(-32.4030462815833,-2.96072985434218,
307.387000891688));
#18527=CARTESIAN_POINT('Ctrl Pts',(-30.534395805612,-0.466043685876077,
307.545912183858));
#18528=CARTESIAN_POINT('Ctrl Pts',(-31.6194936981096,2.45592076268062,307.704823476027));
#18529=CARTESIAN_POINT('Ctrl Pts',(-34.6635002554701,3.12624736533102,307.863734768196));
#18530=CARTESIAN_POINT('Ctrl Pts',(-36.8756086764883,0.930367129504609,
308.022646060366));
#18531=CARTESIAN_POINT('Ctrl Pts',(-36.2277132026935,-2.11849251483108,
308.181557352535));
#18532=CARTESIAN_POINT('Ctrl Pts',(-33.3138175135068,-3.22507535784829,
308.340468644704));
#18533=CARTESIAN_POINT('Ctrl Pts',(-30.8054401339898,-1.37484385937724,
308.499379936874));
#18534=CARTESIAN_POINT('Ctrl Pts',(-31.0023121980512,1.73587230677052,308.658291229043));
#18535=CARTESIAN_POINT('Ctrl Pts',(-33.7239374140105,3.25510561992896,308.817202521212));
#18536=CARTESIAN_POINT('Ctrl Pts',(-36.4750747168593,1.78999223973046,308.976113813381));
#18537=CARTESIAN_POINT('Ctrl Pts',(-36.7334257632008,-1.31622224301346,
309.135025105551));
#18538=CARTESIAN_POINT('Ctrl Pts',(-34.2621290864967,-3.21569754205633,
309.29393639772));
#18539=CARTESIAN_POINT('Ctrl Pts',(-31.3269194820396,-2.16695627088482,
309.452847689889));
#18540=CARTESIAN_POINT('Ctrl Pts',(-30.6188565036962,0.868494353757314,
309.611758982059));
#18541=CARTESIAN_POINT('Ctrl Pts',(-32.7871066163556,3.10769178251591,309.770670274228));
#18542=CARTESIAN_POINT('Ctrl Pts',(-35.8437742462105,2.49769450668719,309.929581566397));
#18543=CARTESIAN_POINT('Ctrl Pts',(-36.9864446642617,-0.402239629036108,
310.088492858567));
#18544=CARTESIAN_POINT('Ctrl Pts',(-35.1674945113613,-2.93339233436557,
310.247404150736));
#18545=CARTESIAN_POINT('Ctrl Pts',(-32.0545740909063,-2.77515159565129,
310.406315442906));
#18546=CARTESIAN_POINT('Ctrl Pts',(-30.5016718282103,-0.0725957243610234,
310.565226735075));
#18547=CARTESIAN_POINT('Ctrl Pts',(-31.9325199384592,2.69651737659405,310.724138027244));
#18548=CARTESIAN_POINT('Ctrl Pts',(-35.0352879222314,2.99340878612678,310.883049319413));
#18549=CARTESIAN_POINT('Ctrl Pts',(-36.9652953162298,0.545882457768805,
311.041960611583));
#18550=CARTESIAN_POINT('Ctrl Pts',(-35.9530722852521,-2.4021199597536,311.200871903752));
#18551=CARTESIAN_POINT('Ctrl Pts',(-32.9266453978538,-3.14781018097909,
311.359783195921));
#18552=CARTESIAN_POINT('Ctrl Pts',(-30.6607040303105,-1.00752436950846,
311.51869448809));
#18553=CARTESIAN_POINT('Ctrl Pts',(-31.2327091352876,2.05648023567375,311.67760578026));
#18554=CARTESIAN_POINT('Ctrl Pts',(-34.1182347323246,3.23506201105244,311.836517072429));
#18555=CARTESIAN_POINT('Ctrl Pts',(-36.6717728395313,1.44767377748021,311.995428364599));
#18556=CARTESIAN_POINT('Ctrl Pts',(-36.5521874844876,-1.66697169850697,
312.154339656768));
#18557=CARTESIAN_POINT('Ctrl Pts',(-33.8691181478586,-3.253302452965,312.313250948937));
#18558=CARTESIAN_POINT('Ctrl Pts',(-31.0824545244631,-1.85694253523434,
312.472162241106));
#18559=CARTESIAN_POINT('Ctrl Pts',(-30.7470716339017,1.24190589362483,312.631073533276));
#18560=CARTESIAN_POINT('Ctrl Pts',(-33.1704437920237,3.20213710348816,312.789984825445));
#18561=CARTESIAN_POINT('Ctrl Pts',(-36.1307987587576,2.2266112950811,312.948896117615));
#18562=CARTESIAN_POINT('Ctrl Pts',(-36.9139715033961,-0.79037417525123,
313.107807409784));
#18563=CARTESIAN_POINT('Ctrl Pts',(-34.802042988206,-3.08260694876516,313.266718701953));
#18564=CARTESIAN_POINT('Ctrl Pts',(-31.7310395895932,-2.54890098558761,
313.425629994122));
#18565=CARTESIAN_POINT('Ctrl Pts',(-30.517011234313,0.322236782390377,313.584541286292));
#18566=CARTESIAN_POINT('Ctrl Pts',(-32.2719552777809,2.89679057424468,313.743452578461));
#18567=CARTESIAN_POINT('Ctrl Pts',(-35.3890868267849,2.81802381861281,313.90236387063));
#18568=CARTESIAN_POINT('Ctrl Pts',(-37.005926459434,0.15030901149958,314.061301785759));
#18569=CARTESIAN_POINT('Ctrl Pts',(-36.100168030815,-1.7105087468349,314.167269270164));
#18570=CARTESIAN_POINT('Ctrl Pts',(-35.3534503877015,-2.24237605679389,
314.220266323846));
#18571=CARTESIAN_POINT('Ctrl Pts',(-35.0467943925255,2.64820704449811,304.002300268831));
#18572=CARTESIAN_POINT('Ctrl Pts',(-35.9281786905302,2.21864321797617,304.055270699554));
#18573=CARTESIAN_POINT('Ctrl Pts',(-37.2121623013899,0.415333579574038,
304.161211561));
#18574=CARTESIAN_POINT('Ctrl Pts',(-35.9776234419694,-2.68533197481934,
304.32012285317));
#18575=CARTESIAN_POINT('Ctrl Pts',(-32.7018869461029,-3.31948752170765,
304.479034145339));
#18576=CARTESIAN_POINT('Ctrl Pts',(-30.3946939051697,-0.912664996122445,
304.637945437508));
#18577=CARTESIAN_POINT('Ctrl Pts',(-31.1683732914037,2.33199542729953,304.796856729678));
#18578=CARTESIAN_POINT('Ctrl Pts',(-34.3150068876391,3.43811615645176,304.955768021847));
#18579=CARTESIAN_POINT('Ctrl Pts',(-36.9490358564228,1.39234645230499,305.114679314016));
#18580=CARTESIAN_POINT('Ctrl Pts',(-36.6558414844005,-1.93006988482577,
305.273590606185));
#18581=CARTESIAN_POINT('Ctrl Pts',(-33.7040830092887,-3.48290475931941,
305.432501898355));
#18582=CARTESIAN_POINT('Ctrl Pts',(-30.8000618131804,-1.84256771683072,
305.591413190524));
#18583=CARTESIAN_POINT('Ctrl Pts',(-30.6062105075215,1.48708478233668,305.750324482693));
#18584=CARTESIAN_POINT('Ctrl Pts',(-33.3002713541492,3.45334216007167,305.909235774863));
#18585=CARTESIAN_POINT('Ctrl Pts',(-36.4122675655127,2.25350826448685,306.068147067032));
#18586=CARTESIAN_POINT('Ctrl Pts',(-37.0890614903658,-1.01238887292895,
306.227058359201));
#18587=CARTESIAN_POINT('Ctrl Pts',(-34.710153141638,-3.35010680903079,306.385969651371));
#18588=CARTESIAN_POINT('Ctrl Pts',(-31.4565745918809,-2.61637932190877,
306.54488094354));
#18589=CARTESIAN_POINT('Ctrl Pts',(-30.3112721244413,0.516097798354423,
306.703792235709));
#18590=CARTESIAN_POINT('Ctrl Pts',(-32.3242823849075,3.17540595195113,306.862703527879));
#18591=CARTESIAN_POINT('Ctrl Pts',(-35.6500367565977,2.92343771002022,307.021614820048));
#18592=CARTESIAN_POINT('Ctrl Pts',(-37.2394163790084,-0.00879738876569104,
307.180526112217));
#18593=CARTESIAN_POINT('Ctrl Pts',(-35.6352458382906,-2.93296685693438,
307.339437404387));
#18594=CARTESIAN_POINT('Ctrl Pts',(-32.3082611520162,-3.16813297065216,
307.498348696556));
#18595=CARTESIAN_POINT('Ctrl Pts',(-30.3087091919254,-0.498690674133233,
307.657259988725));
#18596=CARTESIAN_POINT('Ctrl Pts',(-31.4698196541192,2.62796132181615,307.816171280895));
#18597=CARTESIAN_POINT('Ctrl Pts',(-34.7270629730636,3.34524520634464,307.975082573064));
#18598=CARTESIAN_POINT('Ctrl Pts',(-37.0941325701115,0.995540600731191,
308.133993865233));
#18599=CARTESIAN_POINT('Ctrl Pts',(-36.4008511452441,-2.2668957704712,308.292905157402));
#18600=CARTESIAN_POINT('Ctrl Pts',(-33.2828331361324,-3.45099623292281,
308.451816449572));
#18601=CARTESIAN_POINT('Ctrl Pts',(-30.5987405407777,-1.47115352452833,
308.610727741741));
#18602=CARTESIAN_POINT('Ctrl Pts',(-30.8094037582401,1.85747250119972,308.76963903391));
#18603=CARTESIAN_POINT('Ctrl Pts',(-33.7216824883626,3.48313015533236,308.92855032608));
#18604=CARTESIAN_POINT('Ctrl Pts',(-36.6655406668328,1.91538360839799,309.087461618249));
#18605=CARTESIAN_POINT('Ctrl Pts',(-36.9419895521361,-1.4084253849371,309.246372910419));
#18606=CARTESIAN_POINT('Ctrl Pts',(-34.2975752127978,-3.44096148849664,
309.405284202588));
#18607=CARTESIAN_POINT('Ctrl Pts',(-31.1567502199273,-2.31875447794848,
309.564195494757));
#18608=CARTESIAN_POINT('Ctrl Pts',(-30.3990864757334,0.92933355366023,309.723106786926));
#18609=CARTESIAN_POINT('Ctrl Pts',(-32.7192254308164,3.32538977994698,309.882018079096));
#18610=CARTESIAN_POINT('Ctrl Pts',(-35.9900167474459,2.6726613728866,310.040929371265));
#18611=CARTESIAN_POINT('Ctrl Pts',(-37.212732768196,-0.430417057126371,
310.199840663434));
#18612=CARTESIAN_POINT('Ctrl Pts',(-35.2663627057854,-3.1388804205599,310.358751955604));
#18613=CARTESIAN_POINT('Ctrl Pts',(-31.9353780147653,-2.96955470484632,
310.517663247773));
#18614=CARTESIAN_POINT('Ctrl Pts',(-30.2736928558063,-0.0776811526858028,
310.676574539942));
#18615=CARTESIAN_POINT('Ctrl Pts',(-31.8047738044536,2.8854120527731,310.835485832111));
#18616=CARTESIAN_POINT('Ctrl Pts',(-35.1248948669194,3.20310110564787,310.994397124281));
#18617=CARTESIAN_POINT('Ctrl Pts',(-37.1901018798325,0.584122259591381,
311.15330841645));
#18618=CARTESIAN_POINT('Ctrl Pts',(-36.1069712614174,-2.57039170013971,
311.31221970862));
#18619=CARTESIAN_POINT('Ctrl Pts',(-32.8685390920073,-3.36831852628788,
311.471131000788));
#18620=CARTESIAN_POINT('Ctrl Pts',(-30.4438654779826,-1.07810280937789,
311.630042292958));
#18621=CARTESIAN_POINT('Ctrl Pts',(-31.0559403114233,2.20053944758835,311.788953585127));
#18622=CARTESIAN_POINT('Ctrl Pts',(-34.1436008651973,3.46168246464236,311.947864877297));
#18623=CARTESIAN_POINT('Ctrl Pts',(-36.8760177580772,1.54908527654329,312.106776169466));
#18624=CARTESIAN_POINT('Ctrl Pts',(-36.7480552877541,-1.78374531247374,
312.265687461635));
#18625=CARTESIAN_POINT('Ctrl Pts',(-33.8770333282688,-3.48120067409255,
312.424598753805));
#18626=CARTESIAN_POINT('Ctrl Pts',(-30.8951601626206,-1.98702386232717,
312.583510045974));
#18627=CARTESIAN_POINT('Ctrl Pts',(-30.5362832485983,1.32890307512172,312.742421338143));
#18628=CARTESIAN_POINT('Ctrl Pts',(-33.1294158922425,3.42645112293213,312.901332630312));
#18629=CARTESIAN_POINT('Ctrl Pts',(-36.2971477139041,2.38258841698351,313.060243922482));
#18630=CARTESIAN_POINT('Ctrl Pts',(-37.1351827647435,-0.845740951371512,
313.219155214651));
#18631=CARTESIAN_POINT('Ctrl Pts',(-34.8753108109342,-3.29854771978654,
313.378066506821));
#18632=CARTESIAN_POINT('Ctrl Pts',(-31.5891794856257,-2.72745493464214,
313.53697779899));
#18633=CARTESIAN_POINT('Ctrl Pts',(-30.2901068079786,0.344809903257656,
313.695889091159));
#18634=CARTESIAN_POINT('Ctrl Pts',(-32.1679870467333,3.09971465781636,313.854800383328));
#18635=CARTESIAN_POINT('Ctrl Pts',(-35.5034778615323,3.01543018480285,314.013711675498));
#18636=CARTESIAN_POINT('Ctrl Pts',(-37.2335792893745,0.160838360318353,
314.172649590626));
#18637=CARTESIAN_POINT('Ctrl Pts',(-36.2643712621899,-1.83033218970954,
314.278617075031));
#18638=CARTESIAN_POINT('Ctrl Pts',(-35.4653450418657,-2.39945752149957,
314.331614128713));
#18639=CARTESIAN_POINT('Ctrl Pts',(-35.048294363387,2.64856243216296,314.));
#18640=CARTESIAN_POINT('Ctrl Pts',(-35.1084097821696,2.6123298863998,314.));
#18641=CARTESIAN_POINT('Ctrl Pts',(-35.167002205871,2.5738771597971,314.));
#18642=CARTESIAN_POINT('Ctrl Pts',(-35.2239356243364,2.53320436048268,314.));
#18643=CARTESIAN_POINT('Ctrl Pts',(-35.302523371486,2.4770618741443,314.));
#18644=CARTESIAN_POINT('Ctrl Pts',(-35.3779519219753,2.41669059985685,314.));
#18645=CARTESIAN_POINT('Ctrl Pts',(-35.4500731232314,2.35247138102498,314.));
#18646=CARTESIAN_POINT('Ctrl Pts',(-35.5231270342098,2.28742164510913,314.));
#18647=CARTESIAN_POINT('Ctrl Pts',(-35.5927879602898,2.21842287923684,314.));
#18648=CARTESIAN_POINT('Ctrl Pts',(-35.6588581969503,2.14584033513384,314.));
#18649=CARTESIAN_POINT('Ctrl Pts',(-35.7205977405011,2.07801534510539,314.));
#18650=CARTESIAN_POINT('Ctrl Pts',(-35.7792017240155,2.00706006960028,314.));
#18651=CARTESIAN_POINT('Ctrl Pts',(-35.8344697486721,1.93325966121245,314.));
#18652=CARTESIAN_POINT('Ctrl Pts',(-35.843967544963,1.92057707938679,314.));
#18653=CARTESIAN_POINT('Ctrl Pts',(-35.8533667266025,1.90781045945915,314.));
#18654=CARTESIAN_POINT('Ctrl Pts',(-35.8626661550442,1.89496123542743,314.));
#18655=CARTESIAN_POINT('Ctrl Pts',(-35.8709857286912,1.88346589823451,314.));
#18656=CARTESIAN_POINT('Ctrl Pts',(-35.8792200303602,1.87191193902222,314.));
#18657=CARTESIAN_POINT('Ctrl Pts',(-35.887367573277,1.86030205283278,314.));
#18658=CARTESIAN_POINT('Ctrl Pts',(-35.9425286671464,1.78169994806992,314.));
#18659=CARTESIAN_POINT('Ctrl Pts',(-35.9937329226186,1.70051417088793,314.));
#18660=CARTESIAN_POINT('Ctrl Pts',(-36.0408251356185,1.61710612342277,314.));
#18661=CARTESIAN_POINT('Ctrl Pts',(-36.0877584401856,1.53397952890413,314.));
#18662=CARTESIAN_POINT('Ctrl Pts',(-36.1306077020639,1.4486446755458,314.));
#18663=CARTESIAN_POINT('Ctrl Pts',(-36.1691706243013,1.36144258670802,314.));
#18664=CARTESIAN_POINT('Ctrl Pts',(-36.2068531598979,1.27623131053712,314.));
#18665=CARTESIAN_POINT('Ctrl Pts',(-36.2404429370695,1.18923622578619,314.));
#18666=CARTESIAN_POINT('Ctrl Pts',(-36.2697019974602,1.10077293509858,314.));
#18667=CARTESIAN_POINT('Ctrl Pts',(-36.2828100229337,1.06114148240263,314.));
#18668=CARTESIAN_POINT('Ctrl Pts',(-36.2950481842672,1.02121539777195,314.));
#18669=CARTESIAN_POINT('Ctrl Pts',(-36.3063916868407,0.981023559239999,
314.));
#18670=CARTESIAN_POINT('Ctrl Pts',(-36.3110603578331,0.964481713415173,
314.));
#18671=CARTESIAN_POINT('Ctrl Pts',(-36.3155774556104,0.947894856897153,
314.));
#18672=CARTESIAN_POINT('Ctrl Pts',(-36.3199411435984,0.931265031017353,
314.));
#18673=CARTESIAN_POINT('Ctrl Pts',(-36.3234243468608,0.917990694283236,
314.));
#18674=CARTESIAN_POINT('Ctrl Pts',(-36.3268093077046,0.904690635360945,
314.));
#18675=CARTESIAN_POINT('Ctrl Pts',(-36.3300925197077,0.891377257943442,
314.));
#18676=CARTESIAN_POINT('Ctrl Pts',(-36.3520513927238,0.802334343916824,
314.));
#18677=CARTESIAN_POINT('Ctrl Pts',(-36.3695001180218,0.712556143612094,
314.));
#18678=CARTESIAN_POINT('Ctrl Pts',(-36.3822614546468,0.62235272186204,314.));
#18679=CARTESIAN_POINT('Ctrl Pts',(-36.3946616503746,0.53470202210478,314.));
#18680=CARTESIAN_POINT('Ctrl Pts',(-36.4026359984996,0.446649080643674,
314.));
#18681=CARTESIAN_POINT('Ctrl Pts',(-36.4059737703562,0.358481187047295,
314.));
#18682=CARTESIAN_POINT('Ctrl Pts',(-36.4089167669493,0.280741358916277,
314.));
#18683=CARTESIAN_POINT('Ctrl Pts',(-36.408254518313,0.202911894824171,314.));
#18684=CARTESIAN_POINT('Ctrl Pts',(-36.4038099638934,0.125198274633709,
314.));
#18685=CARTESIAN_POINT('Ctrl Pts',(-36.4008302127494,0.0730969328991553,
314.));
#18686=CARTESIAN_POINT('Ctrl Pts',(-36.3961496017144,0.0210478334846509,
314.));
#18687=CARTESIAN_POINT('Ctrl Pts',(-36.3897974146925,-0.0308821710389396,
314.));
#18688=CARTESIAN_POINT('Ctrl Pts',(-36.387060420309,-0.0532574774058058,
314.));
#18689=CARTESIAN_POINT('Ctrl Pts',(-36.3840130379563,-0.0756106332558332,
314.));
#18690=CARTESIAN_POINT('Ctrl Pts',(-36.3806573700362,-0.0979360923355628,
314.));
#18691=CARTESIAN_POINT('Ctrl Pts',(-36.3784396264198,-0.112690873063438,
314.));
#18692=CARTESIAN_POINT('Ctrl Pts',(-36.3760882417879,-0.12742648365222,
314.));
#18693=CARTESIAN_POINT('Ctrl Pts',(-36.3736056166943,-0.1421336397238,314.));
#18694=CARTESIAN_POINT('Ctrl Pts',(-36.358848312808,-0.229556413308451,
314.));
#18695=CARTESIAN_POINT('Ctrl Pts',(-36.3394450237544,-0.316061693843362,
314.));
#18696=CARTESIAN_POINT('Ctrl Pts',(-36.3156218303925,-0.401349704677867,
314.));
#18697=CARTESIAN_POINT('Ctrl Pts',(-36.2915442390384,-0.487548470774106,
314.));
#18698=CARTESIAN_POINT('Ctrl Pts',(-36.2629512749207,-0.572504691772821,
314.));
#18699=CARTESIAN_POINT('Ctrl Pts',(-36.2300287870974,-0.655885577779074,
314.));
#18700=CARTESIAN_POINT('Ctrl Pts',(-36.2020579810211,-0.726725625027795,
314.));
#18701=CARTESIAN_POINT('Ctrl Pts',(-36.1709610593741,-0.796428449700502,
314.));
#18702=CARTESIAN_POINT('Ctrl Pts',(-36.1368301419288,-0.864770030271797,
314.));
#18703=CARTESIAN_POINT('Ctrl Pts',(-36.1189794373775,-0.900513146913665,
314.));
#18704=CARTESIAN_POINT('Ctrl Pts',(-36.1002985225055,-0.935883572879644,
314.));
#18705=CARTESIAN_POINT('Ctrl Pts',(-36.080798805821,-0.970846733823177,
314.));
#18706=CARTESIAN_POINT('Ctrl Pts',(-36.0694443279123,-0.991205411078644,
314.));
#18707=CARTESIAN_POINT('Ctrl Pts',(-36.0578122052746,-1.01142596615713,
314.));
#18708=CARTESIAN_POINT('Ctrl Pts',(-36.0459045295853,-1.03150126491425,
314.));
#18709=CARTESIAN_POINT('Ctrl Pts',(-36.0381073298707,-1.0446466610288,314.));
#18710=CARTESIAN_POINT('Ctrl Pts',(-36.0301966102719,-1.05772193059368,
314.));
#18711=CARTESIAN_POINT('Ctrl Pts',(-36.0221748813531,-1.07072286206983,
314.));
#18712=CARTESIAN_POINT('Ctrl Pts',(-35.9764975905212,-1.14475270453075,
314.));
#18713=CARTESIAN_POINT('Ctrl Pts',(-35.9272075963404,-1.21640239869884,
314.));
#18714=CARTESIAN_POINT('Ctrl Pts',(-35.8744657309249,-1.28534907412501,
314.));
#18715=CARTESIAN_POINT('Ctrl Pts',(-35.8240263851529,-1.35128578634124,
314.));
#18716=CARTESIAN_POINT('Ctrl Pts',(-35.7704292800472,-1.41475065875741,
314.));
#18717=CARTESIAN_POINT('Ctrl Pts',(-35.7137905242578,-1.47542402497924,
314.));
#18718=CARTESIAN_POINT('Ctrl Pts',(-35.6981895359756,-1.49213633552136,
314.));
#18719=CARTESIAN_POINT('Ctrl Pts',(-35.682357657742,-1.50863661010363,314.));
#18720=CARTESIAN_POINT('Ctrl Pts',(-35.6662970719128,-1.52491759329652,
314.));
#18721=CARTESIAN_POINT('Ctrl Pts',(-35.6500715173412,-1.54136580907671,
314.));
#18722=CARTESIAN_POINT('Ctrl Pts',(-35.6336083386895,-1.55759402253731,
314.));
#18723=CARTESIAN_POINT('Ctrl Pts',(-35.6169334591263,-1.5735723090143,314.));
#18724=CARTESIAN_POINT('Ctrl Pts',(-35.5569485462704,-1.63105135216241,
314.));
#18725=CARTESIAN_POINT('Ctrl Pts',(-35.4941798129402,-1.68534916505214,
314.));
#18726=CARTESIAN_POINT('Ctrl Pts',(-35.428756278306,-1.73615449293592,314.));
#18727=CARTESIAN_POINT('Ctrl Pts',(-35.3640039973732,-1.78643855175975,
314.));
#18728=CARTESIAN_POINT('Ctrl Pts',(-35.2966505706336,-1.83330190156947,
314.));
#18729=CARTESIAN_POINT('Ctrl Pts',(-35.2268031625002,-1.87639577447683,
314.));
#18730=CARTESIAN_POINT('Ctrl Pts',(-35.1960663839232,-1.89535949646701,
314.));
#18731=CARTESIAN_POINT('Ctrl Pts',(-35.1648464609444,-1.91359260343915,
314.));
#18732=CARTESIAN_POINT('Ctrl Pts',(-35.1331518153888,-1.93106208855754,
314.));
#18733=CARTESIAN_POINT('Ctrl Pts',(-35.136256587458,-1.93376001453662,304.));
#18734=CARTESIAN_POINT('Ctrl Pts',(-35.1864755730177,-1.90645007575824,
304.));
#18735=CARTESIAN_POINT('Ctrl Pts',(-35.2355436729036,-1.87725776018492,
304.));
#18736=CARTESIAN_POINT('Ctrl Pts',(-35.2833415381341,-1.8462068102493,304.));
#18737=CARTESIAN_POINT('Ctrl Pts',(-35.3519691462361,-1.80162422453964,
304.));
#18738=CARTESIAN_POINT('Ctrl Pts',(-35.417979523451,-1.75321259707355,304.));
#18739=CARTESIAN_POINT('Ctrl Pts',(-35.4812868793252,-1.70133469307906,
304.));
#18740=CARTESIAN_POINT('Ctrl Pts',(-35.5178418155665,-1.6713793514499,304.));
#18741=CARTESIAN_POINT('Ctrl Pts',(-35.5534952315518,-1.64026732609317,
304.));
#18742=CARTESIAN_POINT('Ctrl Pts',(-35.5882275656708,-1.60806122732678,
304.));
#18743=CARTESIAN_POINT('Ctrl Pts',(-35.6031722450925,-1.59420354014004,
304.));
#18744=CARTESIAN_POINT('Ctrl Pts',(-35.6179463615319,-1.58014323230078,
304.));
#18745=CARTESIAN_POINT('Ctrl Pts',(-35.6325482026628,-1.56588502452514,
304.));
#18746=CARTESIAN_POINT('Ctrl Pts',(-35.6440421171294,-1.55466160282436,
304.));
#18747=CARTESIAN_POINT('Ctrl Pts',(-35.6554289453095,-1.54331576002995,
304.));
#18748=CARTESIAN_POINT('Ctrl Pts',(-35.6666983284761,-1.53185979753453,
304.));
#18749=CARTESIAN_POINT('Ctrl Pts',(-35.7265208404879,-1.47104684585338,
304.));
#18750=CARTESIAN_POINT('Ctrl Pts',(-35.7831066394599,-1.40706632820761,
304.));
#18751=CARTESIAN_POINT('Ctrl Pts',(-35.8363619838647,-1.34030711823897,
304.));
#18752=CARTESIAN_POINT('Ctrl Pts',(-35.8828522774344,-1.28202836134408,
304.));
#18753=CARTESIAN_POINT('Ctrl Pts',(-35.926804443913,-1.22163090931687,304.));
#18754=CARTESIAN_POINT('Ctrl Pts',(-35.9681403014762,-1.15934519918605,
304.));
#18755=CARTESIAN_POINT('Ctrl Pts',(-35.9878823140538,-1.12959753347161,
304.));
#18756=CARTESIAN_POINT('Ctrl Pts',(-36.0070272988542,-1.09941880216891,
304.));
#18757=CARTESIAN_POINT('Ctrl Pts',(-36.0255652755386,-1.06883236996832,
304.));
#18758=CARTESIAN_POINT('Ctrl Pts',(-36.0325711927724,-1.05727307112341,
304.));
#18759=CARTESIAN_POINT('Ctrl Pts',(-36.0394911006069,-1.04565433821461,
304.));
#18760=CARTESIAN_POINT('Ctrl Pts',(-36.0463222172369,-1.03398116891762,
304.));
#18761=CARTESIAN_POINT('Ctrl Pts',(-36.0912572282266,-0.957195188080242,
304.));
#18762=CARTESIAN_POINT('Ctrl Pts',(-36.1322282517761,-0.878271730335654,
304.));
#18763=CARTESIAN_POINT('Ctrl Pts',(-36.169138795271,-0.797614937086259,
304.));
#18764=CARTESIAN_POINT('Ctrl Pts',(-36.2065492466915,-0.715865746749425,
304.));
#18765=CARTESIAN_POINT('Ctrl Pts',(-36.2397891124247,-0.632335215633068,
304.));
#18766=CARTESIAN_POINT('Ctrl Pts',(-36.2687251047273,-0.547401107491553,
304.));
#18767=CARTESIAN_POINT('Ctrl Pts',(-36.2976016694788,-0.462641433528532,
304.));
#18768=CARTESIAN_POINT('Ctrl Pts',(-36.3221925833473,-0.37648307086863,
304.));
#18769=CARTESIAN_POINT('Ctrl Pts',(-36.3423240859166,-0.289271161890286,
304.));
#18770=CARTESIAN_POINT('Ctrl Pts',(-36.3536805126693,-0.240073857671492,
304.));
#18771=CARTESIAN_POINT('Ctrl Pts',(-36.3636170610722,-0.190540814642171,
304.));
#18772=CARTESIAN_POINT('Ctrl Pts',(-36.3720956766504,-0.140731332976591,
304.));
#18773=CARTESIAN_POINT('Ctrl Pts',(-36.3745105282781,-0.126544758910929,
304.));
#18774=CARTESIAN_POINT('Ctrl Pts',(-36.3768074143961,-0.112333537716529,
304.));
#18775=CARTESIAN_POINT('Ctrl Pts',(-36.3789842951394,-0.0981061290234124,
304.));
#18776=CARTESIAN_POINT('Ctrl Pts',(-36.392994413349,-0.00654039754206603,
304.));
#18777=CARTESIAN_POINT('Ctrl Pts',(-36.4019963253058,0.0854153674215651,
304.));
#18778=CARTESIAN_POINT('Ctrl Pts',(-36.405860521369,0.177365179482698,304.));
#18779=CARTESIAN_POINT('Ctrl Pts',(-36.4078070365684,0.223683146747381,
304.));
#18780=CARTESIAN_POINT('Ctrl Pts',(-36.4084492403383,0.270000128814116,
304.));
#18781=CARTESIAN_POINT('Ctrl Pts',(-36.4077662908771,0.316268099145672,
304.));
#18782=CARTESIAN_POINT('Ctrl Pts',(-36.4064446460242,0.405805946854447,
304.));
#18783=CARTESIAN_POINT('Ctrl Pts',(-36.4001638837636,0.495159815679732,
304.));
#18784=CARTESIAN_POINT('Ctrl Pts',(-36.3891755640259,0.584057949482216,
304.));
#18785=CARTESIAN_POINT('Ctrl Pts',(-36.3781872442881,0.6729560832847,304.));
#18786=CARTESIAN_POINT('Ctrl Pts',(-36.3624910987386,0.761399212765894,
304.));
#18787=CARTESIAN_POINT('Ctrl Pts',(-36.3422863391992,0.84911917863751,304.));
#18788=CARTESIAN_POINT('Ctrl Pts',(-36.3370360262829,0.87191367262448,304.));
#18789=CARTESIAN_POINT('Ctrl Pts',(-36.3314810075873,0.894659321429367,
304.));
#18790=CARTESIAN_POINT('Ctrl Pts',(-36.325624234848,0.917351364077548,304.));
#18791=CARTESIAN_POINT('Ctrl Pts',(-36.3220111917182,0.931350085291673,
304.));
#18792=CARTESIAN_POINT('Ctrl Pts',(-36.3182854034492,0.945320190717022,
304.));
#18793=CARTESIAN_POINT('Ctrl Pts',(-36.3144491483228,0.959256442722998,
304.));
#18794=CARTESIAN_POINT('Ctrl Pts',(-36.2899927853656,1.04810090850946,304.));
#18795=CARTESIAN_POINT('Ctrl Pts',(-36.2610373548936,1.13562270896613,304.));
#18796=CARTESIAN_POINT('Ctrl Pts',(-36.2278662880232,1.22154108776326,304.));
#18797=CARTESIAN_POINT('Ctrl Pts',(-36.1936404394721,1.31019152014043,304.));
#18798=CARTESIAN_POINT('Ctrl Pts',(-36.1549265381509,1.39713573522954,304.));
#18799=CARTESIAN_POINT('Ctrl Pts',(-36.1119793205632,1.48206836683025,304.));
#18800=CARTESIAN_POINT('Ctrl Pts',(-36.0690321029756,1.56700099843096,304.));
#18801=CARTESIAN_POINT('Ctrl Pts',(-36.0218512050178,1.64992291753996,304.));
#18802=CARTESIAN_POINT('Ctrl Pts',(-35.9706392647091,1.73051904816679,304.));
#18803=CARTESIAN_POINT('Ctrl Pts',(-35.9398454510111,1.778981617957,304.));
#18804=CARTESIAN_POINT('Ctrl Pts',(-35.90759318223,1.82660302327394,304.));
#18805=CARTESIAN_POINT('Ctrl Pts',(-35.8739182865488,1.87331104247519,304.));
#18806=CARTESIAN_POINT('Ctrl Pts',(-35.8647784686436,1.88598822473753,304.));
#18807=CARTESIAN_POINT('Ctrl Pts',(-35.8555329429828,1.89859915141812,304.));
#18808=CARTESIAN_POINT('Ctrl Pts',(-35.8461934502801,1.91112782045539,304.));
#18809=CARTESIAN_POINT('Ctrl Pts',(-35.7873991537107,1.98999872987687,304.));
#18810=CARTESIAN_POINT('Ctrl Pts',(-35.7247912432541,2.06574291947499,304.));
#18811=CARTESIAN_POINT('Ctrl Pts',(-35.6586401626076,2.13804857623474,304.));
#18812=CARTESIAN_POINT('Ctrl Pts',(-35.5923426775549,2.21051425860013,304.));
#18813=CARTESIAN_POINT('Ctrl Pts',(-35.5224859214325,2.27952707644113,304.));
#18814=CARTESIAN_POINT('Ctrl Pts',(-35.4492921764977,2.34475739531049,304.));
#18815=CARTESIAN_POINT('Ctrl Pts',(-35.3775470541738,2.40869670065248,304.));
#18816=CARTESIAN_POINT('Ctrl Pts',(-35.3025951940527,2.46900251941962,304.));
#18817=CARTESIAN_POINT('Ctrl Pts',(-35.2246051459773,2.52533702182221,304.));
#18818=CARTESIAN_POINT('Ctrl Pts',(-35.1664255709284,2.56736183769632,304.));
#18819=CARTESIAN_POINT('Ctrl Pts',(-35.1065543901557,2.60717614810924,304.));
#18820=CARTESIAN_POINT('Ctrl Pts',(-35.045048879311,2.6446255791971,304.));
#18821=CARTESIAN_POINT('Origin',(-33.7561270252576,0.,304.));
#18822=CARTESIAN_POINT('Ctrl Pts',(-32.4165951196292,2.61935455290103,304.));
#18823=CARTESIAN_POINT('Ctrl Pts',(-32.3729951199972,2.59185154803127,304.));
#18824=CARTESIAN_POINT('Ctrl Pts',(-32.33021699184,2.56313577813171,304.));
#18825=CARTESIAN_POINT('Ctrl Pts',(-32.2883183340065,2.5332036871298,304.));
#18826=CARTESIAN_POINT('Ctrl Pts',(-32.2088386511067,2.47642399001364,304.));
#18827=CARTESIAN_POINT('Ctrl Pts',(-32.1325211106366,2.41526919274723,304.));
#18828=CARTESIAN_POINT('Ctrl Pts',(-32.0595408108092,2.35011684676039,304.));
#18829=CARTESIAN_POINT('Ctrl Pts',(-32.0207536959428,2.31549008400965,304.));
#18830=CARTESIAN_POINT('Ctrl Pts',(-31.982909930747,2.27973359274166,304.));
#18831=CARTESIAN_POINT('Ctrl Pts',(-31.9460408721372,2.24290104434646,304.));
#18832=CARTESIAN_POINT('Ctrl Pts',(-31.9281541386185,2.22503202347093,304.));
#18833=CARTESIAN_POINT('Ctrl Pts',(-31.910496870039,2.20690971360344,304.));
#18834=CARTESIAN_POINT('Ctrl Pts',(-31.8930729674242,2.18854012322945,304.));
#18835=CARTESIAN_POINT('Ctrl Pts',(-31.8768341094174,2.17141989613,304.));
#18836=CARTESIAN_POINT('Ctrl Pts',(-31.8607950118222,2.15408142589293,304.));
#18837=CARTESIAN_POINT('Ctrl Pts',(-31.8449782280288,2.13655141487154,304.));
#18838=CARTESIAN_POINT('Ctrl Pts',(-31.7798728810234,2.06439404928693,304.));
#18839=CARTESIAN_POINT('Ctrl Pts',(-31.7184686521933,1.98893090454704,304.));
#18840=CARTESIAN_POINT('Ctrl Pts',(-31.6609384686365,1.91053545053345,304.));
#18841=CARTESIAN_POINT('Ctrl Pts',(-31.6137878951005,1.84628412382424,304.));
#18842=CARTESIAN_POINT('Ctrl Pts',(-31.5692402724945,1.78006228612976,304.));
#18843=CARTESIAN_POINT('Ctrl Pts',(-31.5274150673336,1.71206593956167,304.));
#18844=CARTESIAN_POINT('Ctrl Pts',(-31.508422782787,1.68118967829326,304.));
#18845=CARTESIAN_POINT('Ctrl Pts',(-31.489992159153,1.64994744210258,304.));
#18846=CARTESIAN_POINT('Ctrl Pts',(-31.4721359899822,1.61835732397993,304.));
#18847=CARTESIAN_POINT('Ctrl Pts',(-31.4616116348991,1.59973823401394,304.));
#18848=CARTESIAN_POINT('Ctrl Pts',(-31.4512868576275,1.58099829230828,304.));
#18849=CARTESIAN_POINT('Ctrl Pts',(-31.4411644485915,1.56214119768984,304.));
#18850=CARTESIAN_POINT('Ctrl Pts',(-31.433918782782,1.54864320474607,304.));
#18851=CARTESIAN_POINT('Ctrl Pts',(-31.4267770469623,1.53508547807366,304.));
#18852=CARTESIAN_POINT('Ctrl Pts',(-31.4197464253918,1.5214817248892,304.));
#18853=CARTESIAN_POINT('Ctrl Pts',(-31.3761638327664,1.43715250488072,304.));
#18854=CARTESIAN_POINT('Ctrl Pts',(-31.3367818849303,1.35093594766862,304.));
#18855=CARTESIAN_POINT('Ctrl Pts',(-31.3017640134589,1.26317540073157,304.));
#18856=CARTESIAN_POINT('Ctrl Pts',(-31.2671097254814,1.17632605384564,304.));
#18857=CARTESIAN_POINT('Ctrl Pts',(-31.2367291567388,1.08796369843067,304.));
#18858=CARTESIAN_POINT('Ctrl Pts',(-31.2108303189363,0.998412005752113,
304.));
#18859=CARTESIAN_POINT('Ctrl Pts',(-31.1856879329934,0.911475934090166,
304.));
#18860=CARTESIAN_POINT('Ctrl Pts',(-31.164769283098,0.823418230371202,304.));
#18861=CARTESIAN_POINT('Ctrl Pts',(-31.1483130220834,0.734538577814548,
304.));
#18862=CARTESIAN_POINT('Ctrl Pts',(-31.1382501561084,0.680189413640112,
304.));
#18863=CARTESIAN_POINT('Ctrl Pts',(-31.1298568208722,0.625533022136213,
304.));
#18864=CARTESIAN_POINT('Ctrl Pts',(-31.1231969611698,0.570640383078611,
304.));
#18865=CARTESIAN_POINT('Ctrl Pts',(-31.120787234397,0.550778664082103,304.));
#18866=CARTESIAN_POINT('Ctrl Pts',(-31.1186040726064,0.530880218793511,
304.));
#18867=CARTESIAN_POINT('Ctrl Pts',(-31.1166536015942,0.510981310296628,
304.));
#18868=CARTESIAN_POINT('Ctrl Pts',(-31.1079529873378,0.422216737087059,
304.));
#18869=CARTESIAN_POINT('Ctrl Pts',(-31.1038634706706,0.333340801037856,
304.));
#18870=CARTESIAN_POINT('Ctrl Pts',(-31.1045676259692,0.244642963201259,
304.));
#18871=CARTESIAN_POINT('Ctrl Pts',(-31.1048840697322,0.204782611901844,
304.));
#18872=CARTESIAN_POINT('Ctrl Pts',(-31.1061693062391,0.164958271719723,
304.));
#18873=CARTESIAN_POINT('Ctrl Pts',(-31.1084433320085,0.12519671516225,304.));
#18874=CARTESIAN_POINT('Ctrl Pts',(-31.1136824223524,0.0335907229086449,
304.));
#18875=CARTESIAN_POINT('Ctrl Pts',(-31.1241665977145,-0.0576836627488685,
304.));
#18876=CARTESIAN_POINT('Ctrl Pts',(-31.1396923668751,-0.148276725180234,
304.));
#18877=CARTESIAN_POINT('Ctrl Pts',(-31.1552181360356,-0.238869787611599,
304.));
#18878=CARTESIAN_POINT('Ctrl Pts',(-31.1757861692824,-0.328782421429016,
304.));
#18879=CARTESIAN_POINT('Ctrl Pts',(-31.2012379505196,-0.41763439700009,
304.));
#18880=CARTESIAN_POINT('Ctrl Pts',(-31.2056830871938,-0.433152335469932,
304.));
#18881=CARTESIAN_POINT('Ctrl Pts',(-31.2102772862545,-0.448637826840731,
304.));
#18882=CARTESIAN_POINT('Ctrl Pts',(-31.2150198204515,-0.464088718625177,
304.));
#18883=CARTESIAN_POINT('Ctrl Pts',(-31.2189504100873,-0.476894343759212,
304.));
#18884=CARTESIAN_POINT('Ctrl Pts',(-31.2229800422566,-0.489666905174659,
304.));
#18885=CARTESIAN_POINT('Ctrl Pts',(-31.2271076474096,-0.502404590095855,
304.));
#18886=CARTESIAN_POINT('Ctrl Pts',(-31.2544438085227,-0.586763290676307,
304.));
#18887=CARTESIAN_POINT('Ctrl Pts',(-31.2860768566243,-0.669605849478574,
304.));
#18888=CARTESIAN_POINT('Ctrl Pts',(-31.3217964375752,-0.750627783818284,
304.));
#18889=CARTESIAN_POINT('Ctrl Pts',(-31.3573807625506,-0.831342920024453,
304.));
#18890=CARTESIAN_POINT('Ctrl Pts',(-31.3970213965721,-0.910251957319242,
304.));
#18891=CARTESIAN_POINT('Ctrl Pts',(-31.4405519276009,-0.987024228084651,
304.));
#18892=CARTESIAN_POINT('Ctrl Pts',(-31.4836967496893,-1.06311624638121,
304.));
#18893=CARTESIAN_POINT('Ctrl Pts',(-31.5306634817197,-1.13710987045192,
304.));
#18894=CARTESIAN_POINT('Ctrl Pts',(-31.581321246188,-1.20864334882212,304.));
#18895=CARTESIAN_POINT('Ctrl Pts',(-31.5986762592469,-1.23315024256868,
304.));
#18896=CARTESIAN_POINT('Ctrl Pts',(-31.6164647169899,-1.25736799689345,
304.));
#18897=CARTESIAN_POINT('Ctrl Pts',(-31.6346820037716,-1.28128076205596,
304.));
#18898=CARTESIAN_POINT('Ctrl Pts',(-31.6453254812064,-1.29525183137379,
304.));
#18899=CARTESIAN_POINT('Ctrl Pts',(-31.6561153448988,-1.30911877942604,
304.));
#18900=CARTESIAN_POINT('Ctrl Pts',(-31.6670507171168,-1.3228783286073,304.));
#18901=CARTESIAN_POINT('Ctrl Pts',(-31.6759908550193,-1.33412735284745,
304.));
#18902=CARTESIAN_POINT('Ctrl Pts',(-31.6850238164214,-1.34529894988918,
304.));
#18903=CARTESIAN_POINT('Ctrl Pts',(-31.6941441122879,-1.3563859440613,304.));
#18904=CARTESIAN_POINT('Ctrl Pts',(-31.7483070899398,-1.4222286125845,304.));
#18905=CARTESIAN_POINT('Ctrl Pts',(-31.8055986639454,-1.48515504772159,
304.));
#18906=CARTESIAN_POINT('Ctrl Pts',(-31.8658620465816,-1.54486745321929,
304.));
#18907=CARTESIAN_POINT('Ctrl Pts',(-31.9251669866202,-1.60363017898558,
304.));
#18908=CARTESIAN_POINT('Ctrl Pts',(-31.9873505939602,-1.65928081190419,
304.));
#18909=CARTESIAN_POINT('Ctrl Pts',(-32.0522893270757,-1.71149313834578,
304.));
#18910=CARTESIAN_POINT('Ctrl Pts',(-32.1151930964543,-1.76206930427372,
304.));
#18911=CARTESIAN_POINT('Ctrl Pts',(-32.1806825889982,-1.80941956418428,
304.));
#18912=CARTESIAN_POINT('Ctrl Pts',(-32.2486612235432,-1.85320170266444,
304.));
#18913=CARTESIAN_POINT('Ctrl Pts',(-32.2911749746431,-1.88058299607264,
304.));
#18914=CARTESIAN_POINT('Ctrl Pts',(-32.3346625680721,-1.90656779027268,
304.));
#18915=CARTESIAN_POINT('Ctrl Pts',(-32.3791022351265,-1.93106208855756,
304.));
#18916=CARTESIAN_POINT('Ctrl Pts',(-32.0470519128079,-2.39933801925114,
303.668487391161));
#18917=CARTESIAN_POINT('Ctrl Pts',(-31.2480517507686,-1.83025205252113,
303.721485292345));
#18918=CARTESIAN_POINT('Ctrl Pts',(-30.2788767558638,0.160810338759522,
303.82745362425));
#18919=CARTESIAN_POINT('Ctrl Pts',(-32.0088834388462,3.01524564186955,303.986392386879));
#18920=CARTESIAN_POINT('Ctrl Pts',(-35.3441694449124,3.09952410938487,304.145303679049));
#18921=CARTESIAN_POINT('Ctrl Pts',(-37.2219347537451,0.34478896869055,304.304214971218));
#18922=CARTESIAN_POINT('Ctrl Pts',(-35.9229416834483,-2.72728782013422,
304.463126263387));
#18923=CARTESIAN_POINT('Ctrl Pts',(-32.6370118643326,-3.2983454038319,304.622037555556));
#18924=CARTESIAN_POINT('Ctrl Pts',(-30.3772784769107,-0.845689126967715,
304.780948847726));
#18925=CARTESIAN_POINT('Ctrl Pts',(-31.2152621400224,2.38244234343232,304.939860139895));
#18926=CARTESIAN_POINT('Ctrl Pts',(-34.3827997320786,3.42624101826296,305.098771432064));
#18927=CARTESIAN_POINT('Ctrl Pts',(-36.9757733735449,1.3288215966872,305.257682724234));
#18928=CARTESIAN_POINT('Ctrl Pts',(-36.6169184655888,-1.98690202842926,
305.416594016403));
#18929=CARTESIAN_POINT('Ctrl Pts',(-33.6352281354669,-3.48098722000116,
305.575505308572));
#18930=CARTESIAN_POINT('Ctrl Pts',(-30.7643822156783,-1.78363594109757,
305.734416600742));
#18931=CARTESIAN_POINT('Ctrl Pts',(-30.6364275912679,1.54899029327215,305.893327892911));
#18932=CARTESIAN_POINT('Ctrl Pts',(-33.3686769436664,3.46147020832407,306.05223918508));
#18933=CARTESIAN_POINT('Ctrl Pts',(-36.456148174692,2.20040451960325,306.21115047725));
#18934=CARTESIAN_POINT('Ctrl Pts',(-37.0681854782468,-1.07803670456918,
306.370061769419));
#18935=CARTESIAN_POINT('Ctrl Pts',(-34.6436605352495,-3.368111994789,306.528973061588));
#18936=CARTESIAN_POINT('Ctrl Pts',(-31.4054269332307,-2.57023409426841,
306.687884353758));
#18937=CARTESIAN_POINT('Ctrl Pts',(-30.3223627279394,0.584086443613537,
306.846795645927));
#18938=CARTESIAN_POINT('Ctrl Pts',(-32.3874431108284,3.20290470461917,307.005706938096));
#18939=CARTESIAN_POINT('Ctrl Pts',(-35.7073605970825,2.88523513113779,307.164618230265));
#18940=CARTESIAN_POINT('Ctrl Pts',(-37.2383476661245,-0.0776763895964064,
307.323529522435));
#18941=CARTESIAN_POINT('Ctrl Pts',(-35.576764394886,-2.96937262392716,307.482440814604));
#18942=CARTESIAN_POINT('Ctrl Pts',(-32.2459839461897,-3.13868795728262,
307.641352106774));
#18943=CARTESIAN_POINT('Ctrl Pts',(-30.2997332272108,-0.430390665717282,
307.800263398942));
#18944=CARTESIAN_POINT('Ctrl Pts',(-31.5223742760276,2.67249749624944,307.959174691112));
#18945=CARTESIAN_POINT('Ctrl Pts',(-34.7929650411445,3.32518588068037,308.118085983281));
#18946=CARTESIAN_POINT('Ctrl Pts',(-37.1129617348198,0.929276570737269,
308.276997275451));
#18947=CARTESIAN_POINT('Ctrl Pts',(-36.3553444474602,-2.31861230143106,
308.43590856762));
#18948=CARTESIAN_POINT('Ctrl Pts',(-33.2147120371004,-3.4407505028467,308.594819859789));
#18949=CARTESIAN_POINT('Ctrl Pts',(-30.5704598424069,-1.40833902606738,
308.753731151959));
#18950=CARTESIAN_POINT('Ctrl Pts',(-30.8468917769978,1.9152661649284,308.912642444128));
#18951=CARTESIAN_POINT('Ctrl Pts',(-33.7905694501548,3.48291658407265,309.071553736297));
#18952=CARTESIAN_POINT('Ctrl Pts',(-36.7026696112863,1.857358608602,309.230465028467));
#18953=CARTESIAN_POINT('Ctrl Pts',(-36.9133199117442,-1.47106331942605,
309.389376320636));
#18954=CARTESIAN_POINT('Ctrl Pts',(-34.2293918939422,-3.45078463198345,
309.548287612805));
#18955=CARTESIAN_POINT('Ctrl Pts',(-31.1115650689105,-2.26675677371728,
309.707198904975));
#18956=CARTESIAN_POINT('Ctrl Pts',(-30.4183261532173,0.99547955826326,309.866110197144));
#18957=CARTESIAN_POINT('Ctrl Pts',(-32.7852506112629,3.34504008962472,310.025021489313));
#18958=CARTESIAN_POINT('Ctrl Pts',(-36.042294209402,2.62780018600281,310.183932781483));
#18959=CARTESIAN_POINT('Ctrl Pts',(-37.2033334770637,-0.498660096465226,
310.342844073652));
#18960=CARTESIAN_POINT('Ctrl Pts',(-35.2039041212998,-3.16793871372917,
310.501755365821));
#18961=CARTESIAN_POINT('Ctrl Pts',(-31.8771234320867,-2.9327870194305,310.660666657991));
#18962=CARTESIAN_POINT('Ctrl Pts',(-30.2730512525257,-0.00879684934994839,
310.81957795016));
#18963=CARTESIAN_POINT('Ctrl Pts',(-31.8623334207013,2.92325845681437,310.978489242329));
#18964=CARTESIAN_POINT('Ctrl Pts',(-35.1878838707564,3.17521124906162,311.137400534498));
#18965=CARTESIAN_POINT('Ctrl Pts',(-37.2007707017131,0.516066153386569,
311.296311826667));
#18966=CARTESIAN_POINT('Ctrl Pts',(-36.0555384594744,-2.61621889632282,
311.455223118837));
#18967=CARTESIAN_POINT('Ctrl Pts',(-32.8021594059117,-3.34990139408307,
311.614134411006));
#18968=CARTESIAN_POINT('Ctrl Pts',(-30.4233969219013,-1.0123267976642,311.773045703176));
#18969=CARTESIAN_POINT('Ctrl Pts',(-31.1001493488858,2.25337008914078,311.931956995345));
#18970=CARTESIAN_POINT('Ctrl Pts',(-34.2119547447221,3.4531304142085,312.090868287514));
#18971=CARTESIAN_POINT('Ctrl Pts',(-36.9058504038466,1.48699360254793,312.249779579683));
#18972=CARTESIAN_POINT('Ctrl Pts',(-36.7120109820576,-1.84245474240054,
312.408690871853));
#18973=CARTESIAN_POINT('Ctrl Pts',(-33.8081678526913,-3.48269119345687,
312.567602164022));
#18974=CARTESIAN_POINT('Ctrl Pts',(-30.8565903603703,-1.9299515573647,312.726513456192));
#18975=CARTESIAN_POINT('Ctrl Pts',(-30.5634139768938,1.39226111162581,312.885424748361));
#18976=CARTESIAN_POINT('Ctrl Pts',(-33.1972814217439,3.43790528342837,313.04433604053));
#18977=CARTESIAN_POINT('Ctrl Pts',(-36.3437220958687,2.33185256123783,313.2032473327));
#18978=CARTESIAN_POINT('Ctrl Pts',(-37.117354034625,-0.912609245665019,
313.362158624869));
#18979=CARTESIAN_POINT('Ctrl Pts',(-34.8103023649712,-3.31928347455001,
313.521069917038));
#18980=CARTESIAN_POINT('Ctrl Pts',(-31.5347668716017,-2.68516768541914,
313.679981209207));
#18981=CARTESIAN_POINT('Ctrl Pts',(-30.3003021687957,0.415311342082169,
313.838892501377));
#18982=CARTESIAN_POINT('Ctrl Pts',(-31.5842082505384,2.21850747685644,313.944833362823));
#18983=CARTESIAN_POINT('Ctrl Pts',(-32.4655386236531,2.64804502178688,313.997803793546));
#18984=CARTESIAN_POINT('Ctrl Pts',(-32.1589359556362,-2.24226614116358,
303.779827133596));
#18985=CARTESIAN_POINT('Ctrl Pts',(-31.4122420776788,-1.71043520097437,
303.832825034778));
#18986=CARTESIAN_POINT('Ctrl Pts',(-30.5065138065885,0.150282942568503,
303.938793366684));
#18987=CARTESIAN_POINT('Ctrl Pts',(-32.1232661683291,2.81785357286398,304.097732129314));
#18988=CARTESIAN_POINT('Ctrl Pts',(-35.240208767702,2.89661477808911,304.256643421483));
#18989=CARTESIAN_POINT('Ctrl Pts',(-36.9950467852155,0.322217471710304,
304.415554713652));
#18990=CARTESIAN_POINT('Ctrl Pts',(-35.7810918710838,-2.54874681567522,
304.574466005822));
#18991=CARTESIAN_POINT('Ctrl Pts',(-32.7102743720378,-3.08242030157264,
304.733377297991));
#18992=CARTESIAN_POINT('Ctrl Pts',(-30.5984736911756,-0.790326365078698,
304.89228859016));
#18993=CARTESIAN_POINT('Ctrl Pts',(-31.3815990280676,2.22647653523201,305.05119988233));
#18994=CARTESIAN_POINT('Ctrl Pts',(-34.3417748084469,3.20194327146731,305.210111174499));
#18995=CARTESIAN_POINT('Ctrl Pts',(-36.7650002791973,1.24183072580518,305.369022466668));
#18996=CARTESIAN_POINT('Ctrl Pts',(-36.4296376903316,-1.85683013748381,
305.527933758838));
#18997=CARTESIAN_POINT('Ctrl Pts',(-33.6431427417149,-3.25310553102805,
305.686845051007));
#18998=CARTESIAN_POINT('Ctrl Pts',(-30.9602358103902,-1.66687079802693,
305.845756343176));
#18999=CARTESIAN_POINT('Ctrl Pts',(-30.8406576935852,1.44758615073306,306.004667635346));
#19000=CARTESIAN_POINT('Ctrl Pts',(-33.394041236439,3.23486619413217,306.163578927515));
#19001=CARTESIAN_POINT('Ctrl Pts',(-36.2793921739056,2.05635575795594,306.322490219684));
#19002=CARTESIAN_POINT('Ctrl Pts',(-36.851362655713,-1.00746338456369,306.481401511853));
#19003=CARTESIAN_POINT('Ctrl Pts',(-34.5855584445221,-3.1476196454885,306.640312804023));
#19004=CARTESIAN_POINT('Ctrl Pts',(-31.5593147453325,-2.40197456056694,
306.799224096192));
#19005=CARTESIAN_POINT('Ctrl Pts',(-30.5471529837359,0.545849415763471,
306.958135388361));
#19006=CARTESIAN_POINT('Ctrl Pts',(-32.4770435552937,2.99322759649458,307.117046680531));
#19007=CARTESIAN_POINT('Ctrl Pts',(-35.5796237299738,2.69635415766267,307.2759579727));
#19008=CARTESIAN_POINT('Ctrl Pts',(-37.0103852316581,-0.0725913301762454,
307.434869264869));
#19009=CARTESIAN_POINT('Ctrl Pts',(-35.4575769654077,-2.77498361702619,
307.593780557039));
#19010=CARTESIAN_POINT('Ctrl Pts',(-32.3448449685662,-2.9332147775032,307.752691849208));
#19011=CARTESIAN_POINT('Ctrl Pts',(-30.5260049158656,-0.402215281660022,
307.911603141377));
#19012=CARTESIAN_POINT('Ctrl Pts',(-31.668606168612,2.49754332240978,308.070514433546));
#19013=CARTESIAN_POINT('Ctrl Pts',(-34.7250887798085,3.10750367538957,308.229425725716));
#19014=CARTESIAN_POINT('Ctrl Pts',(-36.8932076493054,0.868441784201422,
308.388337017885));
#19015=CARTESIAN_POINT('Ctrl Pts',(-36.1851875296823,-2.16682510603776,
308.547248310054));
#19016=CARTESIAN_POINT('Ctrl Pts',(-33.2501555920862,-3.21550289739198,
308.706159602224));
#19017=CARTESIAN_POINT('Ctrl Pts',(-30.779008501811,-1.31614257269836,308.865070894393));
#19018=CARTESIAN_POINT('Ctrl Pts',(-31.0373439102847,1.78988389233944,309.023982186562));
#19019=CARTESIAN_POINT('Ctrl Pts',(-33.7883146880825,3.25490858991212,309.182893478732));
#19020=CARTESIAN_POINT('Ctrl Pts',(-36.5097751653438,1.73576723523384,309.341804770901));
#19021=CARTESIAN_POINT('Ctrl Pts',(-36.7066353128315,-1.37476064072301,
309.50071606307));
#19022=CARTESIAN_POINT('Ctrl Pts',(-34.1984097642212,-3.22488014554912,
309.65962735524));
#19023=CARTESIAN_POINT('Ctrl Pts',(-31.2846904517741,-2.11836428347257,
309.818538647409));
#19024=CARTESIAN_POINT('Ctrl Pts',(-30.6368341947885,0.930310814818372,
309.977449939578));
#19025=CARTESIAN_POINT('Ctrl Pts',(-32.8488087179213,3.12605813504399,310.136361231748));
#19026=CARTESIAN_POINT('Ctrl Pts',(-35.8926310229921,2.45577210694828,310.295272523917));
#19027=CARTESIAN_POINT('Ctrl Pts',(-36.9776632350234,-0.46601547646978,
310.454183816086));
#19028=CARTESIAN_POINT('Ctrl Pts',(-35.1091258675886,-2.96055064275324,
310.613095108255));
#19029=CARTESIAN_POINT('Ctrl Pts',(-32.000131787285,-2.74079307715281,310.772006400425));
#19030=CARTESIAN_POINT('Ctrl Pts',(-30.5010696679198,-0.00822096648659592,
310.930917692594));
#19031=CARTESIAN_POINT('Ctrl Pts',(-31.9863099991538,2.73188829876952,311.089828984763));
#19032=CARTESIAN_POINT('Ctrl Pts',(-35.0941543775033,2.96734708394057,311.248740276933));
#19033=CARTESIAN_POINT('Ctrl Pts',(-36.9752682309223,0.48228205157203,311.407651569102));
#19034=CARTESIAN_POINT('Ctrl Pts',(-35.9050082425686,-2.44494898260645,
311.566562861271));
#19035=CARTESIAN_POINT('Ctrl Pts',(-32.864610583863,-3.13060119579715,311.725474153441));
#19036=CARTESIAN_POINT('Ctrl Pts',(-30.6415730072601,-0.946055155206282,
311.88438544561));
#19037=CARTESIAN_POINT('Ctrl Pts',(-31.2740220581244,2.10585395382022,312.043296737779));
#19038=CARTESIAN_POINT('Ctrl Pts',(-34.1821141322673,3.22707236190863,312.202208029949));
#19039=CARTESIAN_POINT('Ctrl Pts',(-36.6996547938234,1.38964805307454,312.361119322118));
#19040=CARTESIAN_POINT('Ctrl Pts',(-36.518505006335,-1.72183904575499,312.520030614287));
#19041=CARTESIAN_POINT('Ctrl Pts',(-33.8047610169571,-3.25469795441922,
312.678941906457));
#19042=CARTESIAN_POINT('Ctrl Pts',(-31.0464075790711,-1.80360791036664,
312.837853198626));
#19043=CARTESIAN_POINT('Ctrl Pts',(-30.7724238915776,1.30111719366316,312.996764490795));
#19044=CARTESIAN_POINT('Ctrl Pts',(-33.2338660662586,3.21284393933158,313.155675782965));
#19045=CARTESIAN_POINT('Ctrl Pts',(-36.1743260315335,2.17919859657001,313.314587075134));
#19046=CARTESIAN_POINT('Ctrl Pts',(-36.8973124086415,-0.852865580109559,
313.473498367303));
#19047=CARTESIAN_POINT('Ctrl Pts',(-34.7412911214056,-3.10198766834458,
313.632409659472));
#19048=CARTESIAN_POINT('Ctrl Pts',(-31.6801874869731,-2.50938406179264,
313.791320951642));
#19049=CARTESIAN_POINT('Ctrl Pts',(-30.5265366118757,0.388123121010992,
313.950232243811));
#19050=CARTESIAN_POINT('Ctrl Pts',(-31.7263922022207,2.07327361103796,314.056173105257));
#19051=CARTESIAN_POINT('Ctrl Pts',(-32.5500265709333,2.47469162118422,314.10914353598));
#19052=CARTESIAN_POINT('Ctrl Pts',(-32.2708199984643,-2.08519426307603,
303.891166876031));
#19053=CARTESIAN_POINT('Ctrl Pts',(-31.576432404589,-1.59061834942761,303.944164777214));
#19054=CARTESIAN_POINT('Ctrl Pts',(-30.7341508573133,0.139755546377488,
304.050133109119));
#19055=CARTESIAN_POINT('Ctrl Pts',(-32.2376488978119,2.6204615038584,304.209071871748));
#19056=CARTESIAN_POINT('Ctrl Pts',(-35.1362480904917,2.69370544679336,304.367983163918));
#19057=CARTESIAN_POINT('Ctrl Pts',(-36.7681588166858,0.299645974730056,
304.526894456087));
#19058=CARTESIAN_POINT('Ctrl Pts',(-35.6392420587194,-2.37020581121622,
304.685805748256));
#19059=CARTESIAN_POINT('Ctrl Pts',(-32.783536879743,-2.8664951993134,304.844717040425));
#19060=CARTESIAN_POINT('Ctrl Pts',(-30.8196689054406,-0.734963603189685,
305.003628332595));
#19061=CARTESIAN_POINT('Ctrl Pts',(-31.5479359161127,2.07051072703172,305.162539624764));
#19062=CARTESIAN_POINT('Ctrl Pts',(-34.3007498848151,2.97764552467167,305.321450916933));
#19063=CARTESIAN_POINT('Ctrl Pts',(-36.5542271848499,1.15483985492318,305.480362209103));
#19064=CARTESIAN_POINT('Ctrl Pts',(-36.2423569150743,-1.72675824653835,
305.639273501272));
#19065=CARTESIAN_POINT('Ctrl Pts',(-33.6510573479628,-3.02522384205495,
305.798184793441));
#19066=CARTESIAN_POINT('Ctrl Pts',(-31.1560894051021,-1.5501056549563,305.957096085611));
#19067=CARTESIAN_POINT('Ctrl Pts',(-31.0448877959025,1.34618200819396,306.11600737778));
#19068=CARTESIAN_POINT('Ctrl Pts',(-33.4194055292116,3.00826217994027,306.274918669949));
#19069=CARTESIAN_POINT('Ctrl Pts',(-36.1026361731191,1.91230699630863,306.433829962119));
#19070=CARTESIAN_POINT('Ctrl Pts',(-36.6345398331792,-0.936890064558189,
306.592741254288));
#19071=CARTESIAN_POINT('Ctrl Pts',(-34.5274563537948,-2.92712729618799,
306.751652546457));
#19072=CARTESIAN_POINT('Ctrl Pts',(-31.7132025574343,-2.23371502686548,
306.910563838626));
#19073=CARTESIAN_POINT('Ctrl Pts',(-30.7719432395324,0.507612387913404,
307.069475130796));
#19074=CARTESIAN_POINT('Ctrl Pts',(-32.5666439997592,2.78355048836999,307.228386422965));
#19075=CARTESIAN_POINT('Ctrl Pts',(-35.4518868628651,2.50747318418757,307.387297715134));
#19076=CARTESIAN_POINT('Ctrl Pts',(-36.7824227971917,-0.0675062707560861,
307.546209007304));
#19077=CARTESIAN_POINT('Ctrl Pts',(-35.3383895359296,-2.58059461012522,
307.705120299473));
#19078=CARTESIAN_POINT('Ctrl Pts',(-32.4437059909427,-2.72774159772379,
307.864031591642));
#19079=CARTESIAN_POINT('Ctrl Pts',(-30.7522766045202,-0.374039897602761,
308.022942883812));
#19080=CARTESIAN_POINT('Ctrl Pts',(-31.8148380611964,2.32258914857013,308.181854175981));
#19081=CARTESIAN_POINT('Ctrl Pts',(-34.6572125184726,2.88982147009876,308.34076546815));
#19082=CARTESIAN_POINT('Ctrl Pts',(-36.6734535637911,0.807606997665576,
308.49967676032));
#19083=CARTESIAN_POINT('Ctrl Pts',(-36.0150306119043,-2.01503791064446,
308.658588052489));
#19084=CARTESIAN_POINT('Ctrl Pts',(-33.2855991470718,-2.99025529193725,
308.817499344658));
#19085=CARTESIAN_POINT('Ctrl Pts',(-30.9875571612151,-1.22394611932934,
308.976410636827));
#19086=CARTESIAN_POINT('Ctrl Pts',(-31.2277960435716,1.66450161975047,309.135321928997));
#19087=CARTESIAN_POINT('Ctrl Pts',(-33.7860599260102,3.02690059575158,309.294233221166));
#19088=CARTESIAN_POINT('Ctrl Pts',(-36.3168807194012,1.61417586186566,309.453144513335));
#19089=CARTESIAN_POINT('Ctrl Pts',(-36.4999507139187,-1.27845796201997,
309.612055805505));
#19090=CARTESIAN_POINT('Ctrl Pts',(-34.1674276345002,-2.9989756591148,309.770967097674));
#19091=CARTESIAN_POINT('Ctrl Pts',(-31.4578158346379,-1.96997179322788,
309.929878389844));
#19092=CARTESIAN_POINT('Ctrl Pts',(-30.8553422363595,0.86514207137348,310.088789682013));
#19093=CARTESIAN_POINT('Ctrl Pts',(-32.9123668245796,2.90707618046325,310.247700974182));
#19094=CARTESIAN_POINT('Ctrl Pts',(-35.7429678365821,2.28374402789374,310.406612266351));
#19095=CARTESIAN_POINT('Ctrl Pts',(-36.7519929929832,-0.43337085647433,
310.565523558521));
#19096=CARTESIAN_POINT('Ctrl Pts',(-35.0143476138774,-2.75316257177733,
310.72443485069));
#19097=CARTESIAN_POINT('Ctrl Pts',(-32.1231401424832,-2.54879913487514,
310.883346142859));
#19098=CARTESIAN_POINT('Ctrl Pts',(-30.7290880833138,-0.00764508362324373,
311.042257435029));
#19099=CARTESIAN_POINT('Ctrl Pts',(-32.1102865776064,2.54051814072466,311.201168727198));
#19100=CARTESIAN_POINT('Ctrl Pts',(-35.0004248842504,2.75948291881953,311.360080019367));
#19101=CARTESIAN_POINT('Ctrl Pts',(-36.7497657601316,0.448497949757495,
311.518991311536));
#19102=CARTESIAN_POINT('Ctrl Pts',(-35.7544780256626,-2.27367906889009,
311.677902603706));
#19103=CARTESIAN_POINT('Ctrl Pts',(-32.9270617618141,-2.91130099751123,
311.836813895875));
#19104=CARTESIAN_POINT('Ctrl Pts',(-30.8597490926191,-0.879783512748368,
311.995725188045));
#19105=CARTESIAN_POINT('Ctrl Pts',(-31.447894767363,1.95833781849965,312.154636480214));
#19106=CARTESIAN_POINT('Ctrl Pts',(-34.1522735198124,3.00101430960874,312.313547772383));
#19107=CARTESIAN_POINT('Ctrl Pts',(-36.4934591838003,1.29230250360115,312.472459064552));
#19108=CARTESIAN_POINT('Ctrl Pts',(-36.3249990306125,-1.60122334910943,
312.631370356722));
#19109=CARTESIAN_POINT('Ctrl Pts',(-33.801354181223,-3.02670471538159,312.790281648891));
#19110=CARTESIAN_POINT('Ctrl Pts',(-31.2362247977721,-1.67726426336858,
312.949192941061));
#19111=CARTESIAN_POINT('Ctrl Pts',(-30.9814338062613,1.2099732757005,313.10810423323));
#19112=CARTESIAN_POINT('Ctrl Pts',(-33.2704507107733,2.98778259523479,313.267015525399));
#19113=CARTESIAN_POINT('Ctrl Pts',(-36.0049299671983,2.0265446319022,313.425926817568));
#19114=CARTESIAN_POINT('Ctrl Pts',(-36.6772707826581,-0.7931219145541,313.584838109738));
#19115=CARTESIAN_POINT('Ctrl Pts',(-34.6722798778402,-2.88469186213915,
313.743749401907));
#19116=CARTESIAN_POINT('Ctrl Pts',(-31.8256081023445,-2.33360043816614,
313.902660694076));
#19117=CARTESIAN_POINT('Ctrl Pts',(-30.7527710549558,0.360934899939814,
314.061571986246));
#19118=CARTESIAN_POINT('Ctrl Pts',(-31.868576153903,1.92803974521949,314.167512847692));
#19119=CARTESIAN_POINT('Ctrl Pts',(-32.6345145182136,2.30133822058156,314.220483278415));
#19120=CARTESIAN_POINT('Ctrl Pts',(-32.3827040412925,-1.92812238498848,
304.002506618465));
#19121=CARTESIAN_POINT('Ctrl Pts',(-31.7406227314992,-1.47080149788086,
304.055504519648));
#19122=CARTESIAN_POINT('Ctrl Pts',(-30.961787908038,0.129228150186471,304.161472851553));
#19123=CARTESIAN_POINT('Ctrl Pts',(-32.3520316272949,2.42306943485282,304.320411614183));
#19124=CARTESIAN_POINT('Ctrl Pts',(-35.0322874132814,2.49079611549761,304.479322906352));
#19125=CARTESIAN_POINT('Ctrl Pts',(-36.5412708481562,0.277074477749808,
304.638234198521));
#19126=CARTESIAN_POINT('Ctrl Pts',(-35.4973922463549,-2.19166480675722,
304.797145490691));
#19127=CARTESIAN_POINT('Ctrl Pts',(-32.8567993874481,-2.65057009705414,
304.95605678286));
#19128=CARTESIAN_POINT('Ctrl Pts',(-31.0408641197054,-0.679600841300668,
305.114968075029));
#19129=CARTESIAN_POINT('Ctrl Pts',(-31.7142728041579,1.91454491883143,305.273879367199));
#19130=CARTESIAN_POINT('Ctrl Pts',(-34.2597249611834,2.75334777787602,305.432790659368));
#19131=CARTESIAN_POINT('Ctrl Pts',(-36.3434540905024,1.06784898404117,305.591701951537));
#19132=CARTESIAN_POINT('Ctrl Pts',(-36.055076139817,-1.59668635559289,305.750613243707));
#19133=CARTESIAN_POINT('Ctrl Pts',(-33.6589719542107,-2.79734215308184,
305.909524535876));
#19134=CARTESIAN_POINT('Ctrl Pts',(-31.351942999814,-1.43334051188567,306.068435828045));
#19135=CARTESIAN_POINT('Ctrl Pts',(-31.2491178982198,1.24477786565487,306.227347120214));
#19136=CARTESIAN_POINT('Ctrl Pts',(-33.4447698219842,2.78165816574837,306.386258412384));
#19137=CARTESIAN_POINT('Ctrl Pts',(-35.9258801723326,1.76825823466132,306.545169704553));
#19138=CARTESIAN_POINT('Ctrl Pts',(-36.4177170106453,-0.866316744552692,
306.704080996722));
#19139=CARTESIAN_POINT('Ctrl Pts',(-34.4693542630674,-2.7066349468875,306.862992288892));
#19140=CARTESIAN_POINT('Ctrl Pts',(-31.8670903695361,-2.065455493164,307.021903581061));
#19141=CARTESIAN_POINT('Ctrl Pts',(-30.996733495329,0.469375360063339,307.18081487323));
#19142=CARTESIAN_POINT('Ctrl Pts',(-32.6562444442246,2.57387338024539,307.3397261654));
#19143=CARTESIAN_POINT('Ctrl Pts',(-35.3241499957564,2.31859221071245,307.498637457569));
#19144=CARTESIAN_POINT('Ctrl Pts',(-36.5544603627254,-0.0624212113359256,
307.657548749738));
#19145=CARTESIAN_POINT('Ctrl Pts',(-35.2192021064513,-2.38620560322425,
307.816460041908));
#19146=CARTESIAN_POINT('Ctrl Pts',(-32.5425670133193,-2.52226841794439,
307.975371334077));
#19147=CARTESIAN_POINT('Ctrl Pts',(-30.9785482931749,-0.345864513545499,
308.134282626246));
#19148=CARTESIAN_POINT('Ctrl Pts',(-31.9610699537809,2.14763497473048,308.293193918415));
#19149=CARTESIAN_POINT('Ctrl Pts',(-34.5893362571368,2.67213926480795,308.452105210585));
#19150=CARTESIAN_POINT('Ctrl Pts',(-36.4536994782767,0.746772211129729,
308.611016502754));
#19151=CARTESIAN_POINT('Ctrl Pts',(-35.8448736941263,-1.86325071525115,
308.769927794923));
#19152=CARTESIAN_POINT('Ctrl Pts',(-33.3210427020575,-2.76500768648252,
308.928839087093));
#19153=CARTESIAN_POINT('Ctrl Pts',(-31.1961058206193,-1.13174966596031,
309.087750379262));
#19154=CARTESIAN_POINT('Ctrl Pts',(-31.4182481768584,1.53911934716151,309.246661671431));
#19155=CARTESIAN_POINT('Ctrl Pts',(-33.7838051639379,2.79889260159105,309.405572963601));
#19156=CARTESIAN_POINT('Ctrl Pts',(-36.1239862734585,1.49258448849749,309.56448425577));
#19157=CARTESIAN_POINT('Ctrl Pts',(-36.293266115006,-1.18215528331693,309.723395547939));
#19158=CARTESIAN_POINT('Ctrl Pts',(-34.136445504779,-2.77307117268048,309.882306840109));
#19159=CARTESIAN_POINT('Ctrl Pts',(-31.6309412175016,-1.82157930298317,
310.041218132278));
#19160=CARTESIAN_POINT('Ctrl Pts',(-31.0738502779306,0.799973327928591,
310.200129424447));
#19161=CARTESIAN_POINT('Ctrl Pts',(-32.975924931238,2.68809422588251,310.359040716617));
#19162=CARTESIAN_POINT('Ctrl Pts',(-35.5933046501722,2.11171594883921,310.517952008786));
#19163=CARTESIAN_POINT('Ctrl Pts',(-36.526322750943,-0.400726236478883,
310.676863300955));
#19164=CARTESIAN_POINT('Ctrl Pts',(-34.9195693601661,-2.54577450080141,
310.835774593124));
#19165=CARTESIAN_POINT('Ctrl Pts',(-32.2461484976814,-2.35680519259746,
310.994685885294));
#19166=CARTESIAN_POINT('Ctrl Pts',(-30.9571064987078,-0.00706920075989126,
311.153597177463));
#19167=CARTESIAN_POINT('Ctrl Pts',(-32.2342631560589,2.3491479826798,311.312508469633));
#19168=CARTESIAN_POINT('Ctrl Pts',(-34.9066953909973,2.55161875369849,311.471419761802));
#19169=CARTESIAN_POINT('Ctrl Pts',(-36.5242632893408,0.414713847942957,
311.630331053971));
#19170=CARTESIAN_POINT('Ctrl Pts',(-35.6039478087568,-2.10240915517373,
311.78924234614));
#19171=CARTESIAN_POINT('Ctrl Pts',(-32.9895129397654,-2.69200079922531,
311.94815363831));
#19172=CARTESIAN_POINT('Ctrl Pts',(-31.077925177978,-0.813511870290452,
312.107064930479));
#19173=CARTESIAN_POINT('Ctrl Pts',(-31.6217674766015,1.81082168317909,312.265976222648));
#19174=CARTESIAN_POINT('Ctrl Pts',(-34.1224329073576,2.77495625730887,312.424887514818));
#19175=CARTESIAN_POINT('Ctrl Pts',(-36.2872635737771,1.19495695412777,312.583798806987));
#19176=CARTESIAN_POINT('Ctrl Pts',(-36.1314930548899,-1.48060765246388,
312.742710099156));
#19177=CARTESIAN_POINT('Ctrl Pts',(-33.7979473454889,-2.79871147634394,
312.901621391325));
#19178=CARTESIAN_POINT('Ctrl Pts',(-31.426042016473,-1.55092061637053,313.060532683495));
#19179=CARTESIAN_POINT('Ctrl Pts',(-31.1904437209451,1.11882935773785,313.219443975664));
#19180=CARTESIAN_POINT('Ctrl Pts',(-33.307035355288,2.762721251138,313.378355267833));
#19181=CARTESIAN_POINT('Ctrl Pts',(-35.8355339028631,1.8738906672344,313.537266560003));
#19182=CARTESIAN_POINT('Ctrl Pts',(-36.4572291566747,-0.733378248998641,
313.696177852172));
#19183=CARTESIAN_POINT('Ctrl Pts',(-34.6032686342748,-2.66739605593371,
313.855089144342));
#19184=CARTESIAN_POINT('Ctrl Pts',(-31.9710287177159,-2.15781681453964,
314.014000436511));
#19185=CARTESIAN_POINT('Ctrl Pts',(-30.9790054980359,0.333746678868638,
314.17291172868));
#19186=CARTESIAN_POINT('Ctrl Pts',(-32.0107601055854,1.782805879401,314.278852590126));
#19187=CARTESIAN_POINT('Ctrl Pts',(-32.7190024654939,2.1279848199789,314.331823020849));
#19188=CARTESIAN_POINT('',(-32.377264335587,-1.93219025172127,314.001151947217));
#19189=CARTESIAN_POINT('Ctrl Pts',(-32.3759974984059,-1.93375951905296,
314.));
#19190=CARTESIAN_POINT('Ctrl Pts',(-32.3257540111668,-1.90643624108857,
314.));
#19191=CARTESIAN_POINT('Ctrl Pts',(-32.2766866929433,-1.87724182519096,
314.));
#19192=CARTESIAN_POINT('Ctrl Pts',(-32.2289125290216,-1.84620625429721,
314.));
#19193=CARTESIAN_POINT('Ctrl Pts',(-32.1608191978532,-1.80197072543822,
314.));
#19194=CARTESIAN_POINT('Ctrl Pts',(-32.0953516584285,-1.75399746288308,
314.));
#19195=CARTESIAN_POINT('Ctrl Pts',(-32.0325845285674,-1.70265816671701,
314.));
#19196=CARTESIAN_POINT('Ctrl Pts',(-31.9677545339494,-1.6496315857421,314.));
#19197=CARTESIAN_POINT('Ctrl Pts',(-31.9058047707206,-1.59301373041818,
314.));
#19198=CARTESIAN_POINT('Ctrl Pts',(-31.8468374374935,-1.53316100944906,
314.));
#19199=CARTESIAN_POINT('Ctrl Pts',(-31.7880103872424,-1.47345067778871,
314.));
#19200=CARTESIAN_POINT('Ctrl Pts',(-31.7321510803983,-1.41052015262424,
314.));
#19201=CARTESIAN_POINT('Ctrl Pts',(-31.6793887798477,-1.34467971117326,
314.));
#19202=CARTESIAN_POINT('Ctrl Pts',(-31.6703793986152,-1.33343718324413,
314.));
#19203=CARTESIAN_POINT('Ctrl Pts',(-31.6614597242036,-1.32210872662661,
314.));
#19204=CARTESIAN_POINT('Ctrl Pts',(-31.6526411425254,-1.31070993397642,
314.));
#19205=CARTESIAN_POINT('Ctrl Pts',(-31.5997451171298,-1.24233716752603,
314.));
#19206=CARTESIAN_POINT('Ctrl Pts',(-31.5503933030584,-1.17132577496273,
314.));
#19207=CARTESIAN_POINT('Ctrl Pts',(-31.5046726718675,-1.09807055930981,
314.));
#19208=CARTESIAN_POINT('Ctrl Pts',(-31.4576849282052,-1.02278513114822,
314.));
#19209=CARTESIAN_POINT('Ctrl Pts',(-31.4145317574665,-0.945129216982495,
314.));
#19210=CARTESIAN_POINT('Ctrl Pts',(-31.3753363205634,-0.865483493531305,
314.));
#19211=CARTESIAN_POINT('Ctrl Pts',(-31.3361408836603,-0.785837770080116,
314.));
#19212=CARTESIAN_POINT('Ctrl Pts',(-31.3009026029221,-0.70420140232959,
314.));
#19213=CARTESIAN_POINT('Ctrl Pts',(-31.2697822646969,-0.620918813716327,
314.));
#19214=CARTESIAN_POINT('Ctrl Pts',(-31.2557264444749,-0.58330337764046,
314.));
#19215=CARTESIAN_POINT('Ctrl Pts',(-31.2425112341339,-0.545351703294952,
314.));
#19216=CARTESIAN_POINT('Ctrl Pts',(-31.2301544561367,-0.507093809149475,
314.));
#19217=CARTESIAN_POINT('Ctrl Pts',(-31.2260302587649,-0.494324857038999,
314.));
#19218=CARTESIAN_POINT('Ctrl Pts',(-31.2220017037552,-0.481521786356571,
314.));
#19219=CARTESIAN_POINT('Ctrl Pts',(-31.2180695050756,-0.468685693754918,
314.));
#19220=CARTESIAN_POINT('Ctrl Pts',(-31.2137669293524,-0.454640558981847,
314.));
#19221=CARTESIAN_POINT('Ctrl Pts',(-31.2095824026482,-0.44056456576873,
314.));
#19222=CARTESIAN_POINT('Ctrl Pts',(-31.2055177373976,-0.426463984545297,
314.));
#19223=CARTESIAN_POINT('Ctrl Pts',(-31.1801162677167,-0.338344677210859,
314.));
#19224=CARTESIAN_POINT('Ctrl Pts',(-31.159375381469,-0.249211163206453,
314.));
#19225=CARTESIAN_POINT('Ctrl Pts',(-31.1434172941268,-0.15946046529224,
314.));
#19226=CARTESIAN_POINT('Ctrl Pts',(-31.1275109139743,-0.0700005764364917,
314.));
#19227=CARTESIAN_POINT('Ctrl Pts',(-31.1163558477828,0.0200734083628238,
314.));
#19228=CARTESIAN_POINT('Ctrl Pts',(-31.1101146925889,0.110397933079268,
314.));
#19229=CARTESIAN_POINT('Ctrl Pts',(-31.1053794907591,0.178927691020232,
314.));
#19230=CARTESIAN_POINT('Ctrl Pts',(-31.103473686878,0.247602370572859,314.));
#19231=CARTESIAN_POINT('Ctrl Pts',(-31.1044872693873,0.316269774268565,
314.));
#19232=CARTESIAN_POINT('Ctrl Pts',(-31.1053453208484,0.374400380835571,
314.));
#19233=CARTESIAN_POINT('Ctrl Pts',(-31.1082958244446,0.432525934107557,
314.));
#19234=CARTESIAN_POINT('Ctrl Pts',(-31.1132828595529,0.490573353944516,
314.));
#19235=CARTESIAN_POINT('Ctrl Pts',(-31.1146016599839,0.505923749647501,
314.));
#19236=CARTESIAN_POINT('Ctrl Pts',(-31.1160629300108,0.521268682535076,
314.));
#19237=CARTESIAN_POINT('Ctrl Pts',(-31.1176657459376,0.536606800278575,
314.));
#19238=CARTESIAN_POINT('Ctrl Pts',(-31.1191964866191,0.551255195277842,
314.));
#19239=CARTESIAN_POINT('Ctrl Pts',(-31.1208555083163,0.565889202852191,
314.));
#19240=CARTESIAN_POINT('Ctrl Pts',(-31.122640833076,0.580502070227278,314.));
#19241=CARTESIAN_POINT('Ctrl Pts',(-31.1337692874301,0.671588370738572,
314.));
#19242=CARTESIAN_POINT('Ctrl Pts',(-31.1498074944257,0.761920145199774,
314.));
#19243=CARTESIAN_POINT('Ctrl Pts',(-31.1704487043523,0.851206941552089,
314.));
#19244=CARTESIAN_POINT('Ctrl Pts',(-31.191089914279,0.940493737904405,314.));
#19245=CARTESIAN_POINT('Ctrl Pts',(-31.2163344303304,1.02873630292022,314.));
#19246=CARTESIAN_POINT('Ctrl Pts',(-31.2459304858038,1.11565311734405,314.));
#19247=CARTESIAN_POINT('Ctrl Pts',(-31.272566814453,1.19387789416348,314.));
#19248=CARTESIAN_POINT('Ctrl Pts',(-31.302728718844,1.27102932581834,314.));
#19249=CARTESIAN_POINT('Ctrl Pts',(-31.3362676725216,1.34690078032736,314.));
#19250=CARTESIAN_POINT('Ctrl Pts',(-31.3538038375232,1.38657090116585,314.));
#19251=CARTESIAN_POINT('Ctrl Pts',(-31.3722637586092,1.42589103210099,314.));
#19252=CARTESIAN_POINT('Ctrl Pts',(-31.3916295511445,1.4648308304436,314.));
#19253=CARTESIAN_POINT('Ctrl Pts',(-31.4012682821441,1.48421192423163,314.));
#19254=CARTESIAN_POINT('Ctrl Pts',(-31.4111314543575,1.5034987888243,314.));
#19255=CARTESIAN_POINT('Ctrl Pts',(-31.4212170636299,1.52268760355645,314.));
#19256=CARTESIAN_POINT('Ctrl Pts',(-31.4302092303145,1.53979604151892,314.));
#19257=CARTESIAN_POINT('Ctrl Pts',(-31.4393797915133,1.55682916770076,314.));
#19258=CARTESIAN_POINT('Ctrl Pts',(-31.4487149028359,1.57376220373142,314.));
#19259=CARTESIAN_POINT('Ctrl Pts',(-31.4962690987775,1.6600211550678,314.));
#19260=CARTESIAN_POINT('Ctrl Pts',(-31.5481486823058,1.74380084509073,314.));
#19261=CARTESIAN_POINT('Ctrl Pts',(-31.604078655239,1.82477165044164,314.));
#19262=CARTESIAN_POINT('Ctrl Pts',(-31.6600086281722,1.90574245579256,314.));
#19263=CARTESIAN_POINT('Ctrl Pts',(-31.7199894123827,1.98390533447625,314.));
#19264=CARTESIAN_POINT('Ctrl Pts',(-31.7837997715045,2.05891647649168,314.));
#19265=CARTESIAN_POINT('Ctrl Pts',(-31.8048007147617,2.08360376486943,314.));
#19266=CARTESIAN_POINT('Ctrl Pts',(-31.8262168701635,2.10794949134823,314.));
#19267=CARTESIAN_POINT('Ctrl Pts',(-31.8480415044456,2.13194078872289,314.));
#19268=CARTESIAN_POINT('Ctrl Pts',(-31.86386898592,2.14933955975562,314.));
#19269=CARTESIAN_POINT('Ctrl Pts',(-31.879914532835,2.16655510974176,314.));
#19270=CARTESIAN_POINT('Ctrl Pts',(-31.8961553562769,2.18356159119131,314.));
#19271=CARTESIAN_POINT('Ctrl Pts',(-31.9644789868494,2.25510627364289,314.));
#19272=CARTESIAN_POINT('Ctrl Pts',(-32.0363142842366,2.32302056909005,314.));
#19273=CARTESIAN_POINT('Ctrl Pts',(-32.1114230096085,2.38697563761891,314.));
#19274=CARTESIAN_POINT('Ctrl Pts',(-32.1857753014975,2.45028660314906,314.));
#19275=CARTESIAN_POINT('Ctrl Pts',(-32.2633359044913,2.50971853132512,314.));
#19276=CARTESIAN_POINT('Ctrl Pts',(-32.3439167635066,2.56492639140002,314.));
#19277=CARTESIAN_POINT('Ctrl Pts',(-32.3842618400881,2.59256776144546,314.));
#19278=CARTESIAN_POINT('Ctrl Pts',(-32.4253646625726,2.6191497604752,314.));
#19279=CARTESIAN_POINT('Ctrl Pts',(-32.4672051712042,2.64462557919707,314.));
#19280=CARTESIAN_POINT('Ctrl Pts',(-32.4049121771464,-1.94920919778867,
314.));
#19281=CARTESIAN_POINT('Ctrl Pts',(-32.3960384479541,-1.94305782385895,
314.000383982406));
#19282=CARTESIAN_POINT('Ctrl Pts',(-32.3872067253983,-1.93684585282465,
314.000767964811));
#19283=CARTESIAN_POINT('Ctrl Pts',(-32.3784178331262,-1.93057386401469,
314.001151947217));
#19284=CARTESIAN_POINT('Origin',(-33.7561270252576,0.,294.));
#19285=CARTESIAN_POINT('',(-37.7561270252576,4.89858719658941E-16,294.));
#19286=CARTESIAN_POINT('Origin',(-33.7561270252576,0.,294.));
#19287=CARTESIAN_POINT('Origin',(-33.7561270252576,0.,294.));
#19288=CARTESIAN_POINT('',(-37.7561270252576,4.89858719658941E-16,274.));
#19289=CARTESIAN_POINT('Origin',(-33.7561270252576,0.,274.));
#19290=CARTESIAN_POINT('',(-37.7561270252576,4.89858719658941E-16,294.));
#19291=CARTESIAN_POINT('Origin',(-33.7561270252576,0.,274.));
#19292=CARTESIAN_POINT('Origin',(-33.7561270252576,0.,314.));
#19293=CARTESIAN_POINT('',(0.,0.,0.));
#19294=CARTESIAN_POINT('Origin',(-33.7561270252576,0.,309.));
#19295=CARTESIAN_POINT('',(-30.8141270252576,3.60291088309151E-16,309.));
#19296=CARTESIAN_POINT('Origin',(-33.7561270252576,0.,309.));
#19297=CARTESIAN_POINT('',(-30.8141270252576,3.60291088309151E-16,312.));
#19298=CARTESIAN_POINT('',(-30.8141270252576,3.60291088309151E-16,309.));
#19299=CARTESIAN_POINT('Origin',(-33.7561270252576,0.,312.));
#19300=CARTESIAN_POINT('Origin',(-38.3749291787746,8.32667268468867E-16,
309.));
#19301=CARTESIAN_POINT('',(-38.3749291787746,8.32667268468867E-16,309.));
#19302=CARTESIAN_POINT('',(-36.0655281020161,-4.,309.));
#19303=CARTESIAN_POINT('',(-38.3749291787746,8.32667268468867E-16,309.));
#19304=CARTESIAN_POINT('',(-36.0655281020161,-4.,312.));
#19305=CARTESIAN_POINT('',(-36.0655281020161,-4.,309.));
#19306=CARTESIAN_POINT('',(-38.3749291787746,8.32667268468867E-16,312.));
#19307=CARTESIAN_POINT('',(-38.3749291787746,8.32667268468867E-16,312.));
#19308=CARTESIAN_POINT('',(-38.3749291787746,8.32667268468867E-16,309.));
#19309=CARTESIAN_POINT('Origin',(-36.0655281020161,4.,309.));
#19310=CARTESIAN_POINT('',(-36.0655281020161,4.,309.));
#19311=CARTESIAN_POINT('',(-36.0655281020161,4.,309.));
#19312=CARTESIAN_POINT('',(-36.0655281020161,4.,312.));
#19313=CARTESIAN_POINT('',(-36.0655281020161,4.,312.));
#19314=CARTESIAN_POINT('',(-36.0655281020161,4.,309.));
#19315=CARTESIAN_POINT('Origin',(-31.4467259484991,4.,309.));
#19316=CARTESIAN_POINT('',(-31.4467259484991,4.,309.));
#19317=CARTESIAN_POINT('',(-31.4467259484991,4.,309.));
#19318=CARTESIAN_POINT('',(-31.4467259484991,4.,312.));
#19319=CARTESIAN_POINT('',(-31.4467259484991,4.,312.));
#19320=CARTESIAN_POINT('',(-31.4467259484991,4.,309.));
#19321=CARTESIAN_POINT('Origin',(-29.1373248717406,2.77555756156289E-16,
309.));
#19322=CARTESIAN_POINT('',(-29.1373248717406,2.77555756156289E-16,309.));
#19323=CARTESIAN_POINT('',(-29.1373248717406,2.77555756156289E-16,309.));
#19324=CARTESIAN_POINT('',(-29.1373248717406,2.77555756156289E-16,312.));
#19325=CARTESIAN_POINT('',(-29.1373248717406,2.77555756156289E-16,312.));
#19326=CARTESIAN_POINT('',(-29.1373248717406,2.77555756156289E-16,309.));
#19327=CARTESIAN_POINT('Origin',(-31.4467259484991,-4.,309.));
#19328=CARTESIAN_POINT('',(-31.4467259484991,-4.,309.));
#19329=CARTESIAN_POINT('',(-31.4467259484991,-4.,309.));
#19330=CARTESIAN_POINT('',(-31.4467259484991,-4.,312.));
#19331=CARTESIAN_POINT('',(-31.4467259484991,-4.,312.));
#19332=CARTESIAN_POINT('',(-31.4467259484991,-4.,309.));
#19333=CARTESIAN_POINT('Origin',(-36.0655281020161,-4.,309.));
#19334=CARTESIAN_POINT('',(-36.0655281020161,-4.,309.));
#19335=CARTESIAN_POINT('',(-36.0655281020161,-4.,312.));
#19336=CARTESIAN_POINT('Origin',(-33.7561270252576,5.55111512312578E-16,
312.));
#19337=CARTESIAN_POINT('Origin',(-33.7561270252576,5.55111512312578E-16,
309.));
#19338=CARTESIAN_POINT('',(0.,0.,0.));
#19339=CARTESIAN_POINT('Origin',(0.,0.,0.));
#19340=CARTESIAN_POINT('',(-5.44687084534895,-5.85931719521034,0.));
#19341=CARTESIAN_POINT('',(5.44687084534894,-5.85931719521034,0.));
#19342=CARTESIAN_POINT('',(-17.7281904880723,-5.85931719521034,0.));
#19343=CARTESIAN_POINT('Origin',(0.,0.,0.));
#19344=CARTESIAN_POINT('Origin',(0.,0.,0.));
#19345=CARTESIAN_POINT('',(5.44687084534895,5.85931719521034,0.));
#19346=CARTESIAN_POINT('',(-5.44687084534894,5.85931719521034,0.));
#19347=CARTESIAN_POINT('',(17.7281904880723,5.85931719521034,0.));
#19348=CARTESIAN_POINT('Origin',(0.,0.,0.));
#19349=CARTESIAN_POINT('Origin',(0.,0.,7.));
#19350=CARTESIAN_POINT('',(-8.,9.79717439317882E-16,7.));
#19351=CARTESIAN_POINT('Origin',(0.,0.,7.));
#19352=CARTESIAN_POINT('Origin',(5.44687084534894,-5.85931719521034,0.));
#19353=CARTESIAN_POINT('',(-5.44687084534895,-5.85931719521034,-21.));
#19354=CARTESIAN_POINT('',(-5.44687084534895,-5.85931719521034,0.));
#19355=CARTESIAN_POINT('',(5.44687084534894,-5.85931719521034,-21.));
#19356=CARTESIAN_POINT('',(-17.7281904880723,-5.85931719521034,-21.));
#19357=CARTESIAN_POINT('',(5.44687084534894,-5.85931719521034,0.));
#19358=CARTESIAN_POINT('Origin',(0.,0.,0.));
#19359=CARTESIAN_POINT('',(-8.,9.79717439317883E-16,-21.));
#19360=CARTESIAN_POINT('Origin',(0.,0.,-21.));
#19361=CARTESIAN_POINT('',(5.44687084534895,5.85931719521034,-21.));
#19362=CARTESIAN_POINT('Origin',(0.,0.,-21.));
#19363=CARTESIAN_POINT('',(5.44687084534895,5.85931719521034,0.));
#19364=CARTESIAN_POINT('',(-5.44687084534894,5.85931719521034,-21.));
#19365=CARTESIAN_POINT('',(-5.44687084534894,5.85931719521034,0.));
#19366=CARTESIAN_POINT('Origin',(0.,0.,-21.));
#19367=CARTESIAN_POINT('',(-8.,9.79717439317883E-16,0.));
#19368=CARTESIAN_POINT('Origin',(-5.44687084534894,5.85931719521034,0.));
#19369=CARTESIAN_POINT('',(17.7281904880723,5.85931719521034,-21.));
#19370=CARTESIAN_POINT('Origin',(0.,0.,-21.));
#19371=CARTESIAN_POINT('',(0.,0.,0.));
#19372=CARTESIAN_POINT('Origin',(0.,0.,307.));
#19373=CARTESIAN_POINT('',(-3.933,4.81653586104654E-16,307.));
#19374=CARTESIAN_POINT('Origin',(0.,0.,307.));
#19375=CARTESIAN_POINT('',(-3.933,4.81653586104654E-16,302.));
#19376=CARTESIAN_POINT('',(-3.933,4.81653586104654E-16,307.));
#19377=CARTESIAN_POINT('Origin',(0.,0.,302.));
#19378=CARTESIAN_POINT('Origin',(-6.75523463248397,-4.9960036108132E-15,
307.));
#19379=CARTESIAN_POINT('',(-6.75523463248397,-4.9960036108132E-15,307.));
#19380=CARTESIAN_POINT('',(-3.37761731624199,5.85020480025555,307.));
#19381=CARTESIAN_POINT('',(-6.75523463248397,-4.9960036108132E-15,307.));
#19382=CARTESIAN_POINT('',(-3.37761731624199,5.85020480025555,302.));
#19383=CARTESIAN_POINT('',(-3.37761731624199,5.85020480025555,307.));
#19384=CARTESIAN_POINT('',(-6.75523463248397,-4.9960036108132E-15,302.));
#19385=CARTESIAN_POINT('',(-6.75523463248397,-4.9960036108132E-15,302.));
#19386=CARTESIAN_POINT('',(-6.75523463248397,-4.9960036108132E-15,307.));
#19387=CARTESIAN_POINT('Origin',(-3.37761731624198,-5.85020480025556,307.));
#19388=CARTESIAN_POINT('',(-3.37761731624198,-5.85020480025556,307.));
#19389=CARTESIAN_POINT('',(-3.37761731624198,-5.85020480025556,307.));
#19390=CARTESIAN_POINT('',(-3.37761731624198,-5.85020480025556,302.));
#19391=CARTESIAN_POINT('',(-3.37761731624198,-5.85020480025556,302.));
#19392=CARTESIAN_POINT('',(-3.37761731624198,-5.85020480025556,307.));
#19393=CARTESIAN_POINT('Origin',(3.37761731624199,-5.85020480025555,307.));
#19394=CARTESIAN_POINT('',(3.37761731624199,-5.85020480025555,307.));
#19395=CARTESIAN_POINT('',(3.37761731624199,-5.85020480025555,307.));
#19396=CARTESIAN_POINT('',(3.37761731624199,-5.85020480025555,302.));
#19397=CARTESIAN_POINT('',(3.37761731624199,-5.85020480025555,302.));
#19398=CARTESIAN_POINT('',(3.37761731624199,-5.85020480025555,307.));
#19399=CARTESIAN_POINT('Origin',(6.75523463248397,2.77555756156289E-15,
307.));
#19400=CARTESIAN_POINT('',(6.75523463248397,2.77555756156289E-15,307.));
#19401=CARTESIAN_POINT('',(6.75523463248397,2.77555756156289E-15,307.));
#19402=CARTESIAN_POINT('',(6.75523463248397,2.77555756156289E-15,302.));
#19403=CARTESIAN_POINT('',(6.75523463248397,2.77555756156289E-15,302.));
#19404=CARTESIAN_POINT('',(6.75523463248397,2.77555756156289E-15,307.));
#19405=CARTESIAN_POINT('Origin',(3.37761731624198,5.85020480025556,307.));
#19406=CARTESIAN_POINT('',(3.37761731624198,5.85020480025556,307.));
#19407=CARTESIAN_POINT('',(3.37761731624198,5.85020480025556,307.));
#19408=CARTESIAN_POINT('',(3.37761731624198,5.85020480025556,302.));
#19409=CARTESIAN_POINT('',(3.37761731624198,5.85020480025556,302.));
#19410=CARTESIAN_POINT('',(3.37761731624198,5.85020480025556,307.));
#19411=CARTESIAN_POINT('Origin',(-3.37761731624199,5.85020480025555,307.));
#19412=CARTESIAN_POINT('',(-3.37761731624199,5.85020480025555,307.));
#19413=CARTESIAN_POINT('',(-3.37761731624199,5.85020480025555,302.));
#19414=CARTESIAN_POINT('Origin',(0.,0.,302.));
#19415=CARTESIAN_POINT('Origin',(0.,0.,307.));
#19416=CARTESIAN_POINT('',(0.,0.,0.));
#19417=CARTESIAN_POINT('',(0.,0.,0.));
#19418=CARTESIAN_POINT('',(0.,0.,0.));
#19419=CARTESIAN_POINT('',(0.,0.,0.));
#19420=CARTESIAN_POINT('',(0.,0.,0.));
#19421=CARTESIAN_POINT('',(0.,0.,0.));
#19422=CARTESIAN_POINT('',(0.,0.,0.));
#19423=CARTESIAN_POINT('',(0.,0.,0.));
#19424=UNCERTAINTY_MEASURE_WITH_UNIT(LENGTH_MEASURE(0.01),#19444,
'DISTANCE_ACCURACY_VALUE',
'Maximum model space distance between geometric entities at asserted c
onnectivities');
#19425=UNCERTAINTY_MEASURE_WITH_UNIT(LENGTH_MEASURE(0.01),#19444,
'DISTANCE_ACCURACY_VALUE',
'Maximum model space distance between geometric entities at asserted c
onnectivities');
#19426=UNCERTAINTY_MEASURE_WITH_UNIT(LENGTH_MEASURE(0.01),#19444,
'DISTANCE_ACCURACY_VALUE',
'Maximum model space distance between geometric entities at asserted c
onnectivities');
#19427=UNCERTAINTY_MEASURE_WITH_UNIT(LENGTH_MEASURE(0.01),#19444,
'DISTANCE_ACCURACY_VALUE',
'Maximum model space distance between geometric entities at asserted c
onnectivities');
#19428=UNCERTAINTY_MEASURE_WITH_UNIT(LENGTH_MEASURE(0.01),#19444,
'DISTANCE_ACCURACY_VALUE',
'Maximum model space distance between geometric entities at asserted c
onnectivities');
#19429=UNCERTAINTY_MEASURE_WITH_UNIT(LENGTH_MEASURE(0.01),#19444,
'DISTANCE_ACCURACY_VALUE',
'Maximum model space distance between geometric entities at asserted c
onnectivities');
#19430=UNCERTAINTY_MEASURE_WITH_UNIT(LENGTH_MEASURE(0.01),#19444,
'DISTANCE_ACCURACY_VALUE',
'Maximum model space distance between geometric entities at asserted c
onnectivities');
#19431=UNCERTAINTY_MEASURE_WITH_UNIT(LENGTH_MEASURE(0.01),#19444,
'DISTANCE_ACCURACY_VALUE',
'Maximum model space distance between geometric entities at asserted c
onnectivities');
#19432=UNCERTAINTY_MEASURE_WITH_UNIT(LENGTH_MEASURE(0.01),#19444,
'DISTANCE_ACCURACY_VALUE',
'Maximum model space distance between geometric entities at asserted c
onnectivities');
#19433=UNCERTAINTY_MEASURE_WITH_UNIT(LENGTH_MEASURE(0.01),#19444,
'DISTANCE_ACCURACY_VALUE',
'Maximum model space distance between geometric entities at asserted c
onnectivities');
#19434=(
GEOMETRIC_REPRESENTATION_CONTEXT(3)
GLOBAL_UNCERTAINTY_ASSIGNED_CONTEXT((#19424))
GLOBAL_UNIT_ASSIGNED_CONTEXT((#19444,#19446,#19447))
REPRESENTATION_CONTEXT('','3D')
);
#19435=(
GEOMETRIC_REPRESENTATION_CONTEXT(3)
GLOBAL_UNCERTAINTY_ASSIGNED_CONTEXT((#19425))
GLOBAL_UNIT_ASSIGNED_CONTEXT((#19444,#19446,#19447))
REPRESENTATION_CONTEXT('','3D')
);
#19436=(
GEOMETRIC_REPRESENTATION_CONTEXT(3)
GLOBAL_UNCERTAINTY_ASSIGNED_CONTEXT((#19426))
GLOBAL_UNIT_ASSIGNED_CONTEXT((#19444,#19446,#19447))
REPRESENTATION_CONTEXT('','3D')
);
#19437=(
GEOMETRIC_REPRESENTATION_CONTEXT(3)
GLOBAL_UNCERTAINTY_ASSIGNED_CONTEXT((#19427))
GLOBAL_UNIT_ASSIGNED_CONTEXT((#19444,#19446,#19447))
REPRESENTATION_CONTEXT('','3D')
);
#19438=(
GEOMETRIC_REPRESENTATION_CONTEXT(3)
GLOBAL_UNCERTAINTY_ASSIGNED_CONTEXT((#19428))
GLOBAL_UNIT_ASSIGNED_CONTEXT((#19444,#19446,#19447))
REPRESENTATION_CONTEXT('','3D')
);
#19439=(
GEOMETRIC_REPRESENTATION_CONTEXT(3)
GLOBAL_UNCERTAINTY_ASSIGNED_CONTEXT((#19429))
GLOBAL_UNIT_ASSIGNED_CONTEXT((#19444,#19446,#19447))
REPRESENTATION_CONTEXT('','3D')
);
#19440=(
GEOMETRIC_REPRESENTATION_CONTEXT(3)
GLOBAL_UNCERTAINTY_ASSIGNED_CONTEXT((#19430))
GLOBAL_UNIT_ASSIGNED_CONTEXT((#19444,#19446,#19447))
REPRESENTATION_CONTEXT('','3D')
);
#19441=(
GEOMETRIC_REPRESENTATION_CONTEXT(3)
GLOBAL_UNCERTAINTY_ASSIGNED_CONTEXT((#19431))
GLOBAL_UNIT_ASSIGNED_CONTEXT((#19444,#19446,#19447))
REPRESENTATION_CONTEXT('','3D')
);
#19442=(
GEOMETRIC_REPRESENTATION_CONTEXT(3)
GLOBAL_UNCERTAINTY_ASSIGNED_CONTEXT((#19432))
GLOBAL_UNIT_ASSIGNED_CONTEXT((#19444,#19446,#19447))
REPRESENTATION_CONTEXT('','3D')
);
#19443=(
GEOMETRIC_REPRESENTATION_CONTEXT(3)
GLOBAL_UNCERTAINTY_ASSIGNED_CONTEXT((#19433))
GLOBAL_UNIT_ASSIGNED_CONTEXT((#19444,#19446,#19447))
REPRESENTATION_CONTEXT('','3D')
);
#19444=(
LENGTH_UNIT()
NAMED_UNIT(*)
SI_UNIT(.MILLI.,.METRE.)
);
#19445=(
LENGTH_UNIT()
NAMED_UNIT(*)
SI_UNIT($,.METRE.)
);
#19446=(
NAMED_UNIT(*)
PLANE_ANGLE_UNIT()
SI_UNIT($,.RADIAN.)
);
#19447=(
NAMED_UNIT(*)
SI_UNIT($,.STERADIAN.)
SOLID_ANGLE_UNIT()
);
#19448=SHAPE_DEFINITION_REPRESENTATION(#19457,#19474);
#19449=SHAPE_DEFINITION_REPRESENTATION(#19458,#19475);
#19450=SHAPE_DEFINITION_REPRESENTATION(#19459,#19476);
#19451=SHAPE_DEFINITION_REPRESENTATION(#19460,#19477);
#19452=SHAPE_DEFINITION_REPRESENTATION(#19461,#19478);
#19453=SHAPE_DEFINITION_REPRESENTATION(#19462,#19479);
#19454=SHAPE_DEFINITION_REPRESENTATION(#19463,#19480);
#19455=SHAPE_DEFINITION_REPRESENTATION(#19464,#19481);
#19456=SHAPE_DEFINITION_REPRESENTATION(#19465,#19482);
#19457=PRODUCT_DEFINITION_SHAPE('',$,#19484);
#19458=PRODUCT_DEFINITION_SHAPE('',$,#19485);
#19459=PRODUCT_DEFINITION_SHAPE('',$,#19486);
#19460=PRODUCT_DEFINITION_SHAPE('',$,#19487);
#19461=PRODUCT_DEFINITION_SHAPE('',$,#19488);
#19462=PRODUCT_DEFINITION_SHAPE('',$,#19489);
#19463=PRODUCT_DEFINITION_SHAPE('',$,#19490);
#19464=PRODUCT_DEFINITION_SHAPE('',$,#19491);
#19465=PRODUCT_DEFINITION_SHAPE('',$,#19492);
#19466=PRODUCT_DEFINITION_SHAPE($,$,#35);
#19467=PRODUCT_DEFINITION_SHAPE($,$,#36);
#19468=PRODUCT_DEFINITION_SHAPE($,$,#37);
#19469=PRODUCT_DEFINITION_SHAPE($,$,#38);
#19470=PRODUCT_DEFINITION_SHAPE($,$,#39);
#19471=PRODUCT_DEFINITION_SHAPE($,$,#40);
#19472=PRODUCT_DEFINITION_SHAPE($,$,#41);
#19473=PRODUCT_DEFINITION_SHAPE($,$,#42);
#19474=SHAPE_REPRESENTATION('',(#2115,#2258,#2259,#2260,#2261,#2262,#2263,
#2264,#2265),#19434);
#19475=SHAPE_REPRESENTATION('',(#2116),#19435);
#19476=SHAPE_REPRESENTATION('',(#2125),#19436);
#19477=SHAPE_REPRESENTATION('',(#2131),#19437);
#19478=SHAPE_REPRESENTATION('',(#2150),#19438);
#19479=SHAPE_REPRESENTATION('',(#2195),#19439);
#19480=SHAPE_REPRESENTATION('',(#2220),#19440);
#19481=SHAPE_REPRESENTATION('',(#2232),#19441);
#19482=SHAPE_REPRESENTATION('',(#2246),#19442);
#19483=PRODUCT_DEFINITION_CONTEXT('part definition',#19512,'design');
#19484=PRODUCT_DEFINITION('BR-108','BR-108',#19493,#19483);
#19485=PRODUCT_DEFINITION('Cylinder','Cylinder',#19494,#19483);
#19486=PRODUCT_DEFINITION('Sealing','Sealing',#19495,#19483);
#19487=PRODUCT_DEFINITION('Rod','Rod',#19496,#19483);
#19488=PRODUCT_DEFINITION('Clamp','Clamp',#19497,#19483);
#19489=PRODUCT_DEFINITION('Screw','Screw',#19498,#19483);
#19490=PRODUCT_DEFINITION('Nut_01','Nut_01',#19499,#19483);
#19491=PRODUCT_DEFINITION('Pin','Pin',#19500,#19483);
#19492=PRODUCT_DEFINITION('Nut_02','Nut_02',#19501,#19483);
#19493=PRODUCT_DEFINITION_FORMATION('',$,#19514);
#19494=PRODUCT_DEFINITION_FORMATION('',$,#19515);
#19495=PRODUCT_DEFINITION_FORMATION('',$,#19516);
#19496=PRODUCT_DEFINITION_FORMATION('',$,#19517);
#19497=PRODUCT_DEFINITION_FORMATION('',$,#19518);
#19498=PRODUCT_DEFINITION_FORMATION('',$,#19519);
#19499=PRODUCT_DEFINITION_FORMATION('',$,#19520);
#19500=PRODUCT_DEFINITION_FORMATION('',$,#19521);
#19501=PRODUCT_DEFINITION_FORMATION('',$,#19522);
#19502=PRODUCT_RELATED_PRODUCT_CATEGORY('BR-108','BR-108',(#19514));
#19503=PRODUCT_RELATED_PRODUCT_CATEGORY('Cylinder','Cylinder',(#19515));
#19504=PRODUCT_RELATED_PRODUCT_CATEGORY('Sealing','Sealing',(#19516));
#19505=PRODUCT_RELATED_PRODUCT_CATEGORY('Rod','Rod',(#19517));
#19506=PRODUCT_RELATED_PRODUCT_CATEGORY('Clamp','Clamp',(#19518));
#19507=PRODUCT_RELATED_PRODUCT_CATEGORY('Screw','Screw',(#19519));
#19508=PRODUCT_RELATED_PRODUCT_CATEGORY('Nut_01','Nut_01',(#19520));
#19509=PRODUCT_RELATED_PRODUCT_CATEGORY('Pin','Pin',(#19521));
#19510=PRODUCT_RELATED_PRODUCT_CATEGORY('Nut_02','Nut_02',(#19522));
#19511=APPLICATION_PROTOCOL_DEFINITION('international standard',
'automotive_design',2009,#19512);
#19512=APPLICATION_CONTEXT(
'Core Data for Automotive Mechanical Design Process');
#19513=PRODUCT_CONTEXT('part definition',#19512,'mechanical');
#19514=PRODUCT('BR-108','BR-108',$,(#19513));
#19515=PRODUCT('Cylinder','Cylinder',$,(#19513));
#19516=PRODUCT('Sealing','Sealing',$,(#19513));
#19517=PRODUCT('Rod','Rod',$,(#19513));
#19518=PRODUCT('Clamp','Clamp',$,(#19513));
#19519=PRODUCT('Screw','Screw',$,(#19513));
#19520=PRODUCT('Nut_01','Nut_01',$,(#19513));
#19521=PRODUCT('Pin','Pin',$,(#19513));
#19522=PRODUCT('Nut_02','Nut_02',$,(#19513));
#19523=PRESENTATION_STYLE_ASSIGNMENT((#19526));
#19524=PRESENTATION_STYLE_ASSIGNMENT((#19527));
#19525=PRESENTATION_STYLE_ASSIGNMENT((#19528));
#19526=SURFACE_STYLE_USAGE(.BOTH.,#19529);
#19527=SURFACE_STYLE_USAGE(.BOTH.,#19530);
#19528=SURFACE_STYLE_USAGE(.BOTH.,#19531);
#19529=SURFACE_SIDE_STYLE('',(#19532));
#19530=SURFACE_SIDE_STYLE('',(#19533));
#19531=SURFACE_SIDE_STYLE('',(#19534));
#19532=SURFACE_STYLE_FILL_AREA(#19535);
#19533=SURFACE_STYLE_FILL_AREA(#19536);
#19534=SURFACE_STYLE_FILL_AREA(#19537);
#19535=FILL_AREA_STYLE('Steel - Satin',(#19538));
#19536=FILL_AREA_STYLE('Opaque(36,31,37)',(#19539));
#19537=FILL_AREA_STYLE('Opaque(160,160,160)',(#19540));
#19538=FILL_AREA_STYLE_COLOUR('Steel - Satin',#19541);
#19539=FILL_AREA_STYLE_COLOUR('Opaque(36,31,37)',#19542);
#19540=FILL_AREA_STYLE_COLOUR('Opaque(160,160,160)',#19543);
#19541=COLOUR_RGB('Steel - Satin',0.627450980392157,0.627450980392157,0.627450980392157);
#19542=COLOUR_RGB('Opaque(36,31,37)',0.141176470588235,0.12156862745098,
0.145098039215686);
#19543=COLOUR_RGB('Opaque(160,160,160)',0.627450980392157,0.627450980392157,
0.627450980392157);
ENDSEC;
END-ISO-10303-21;
